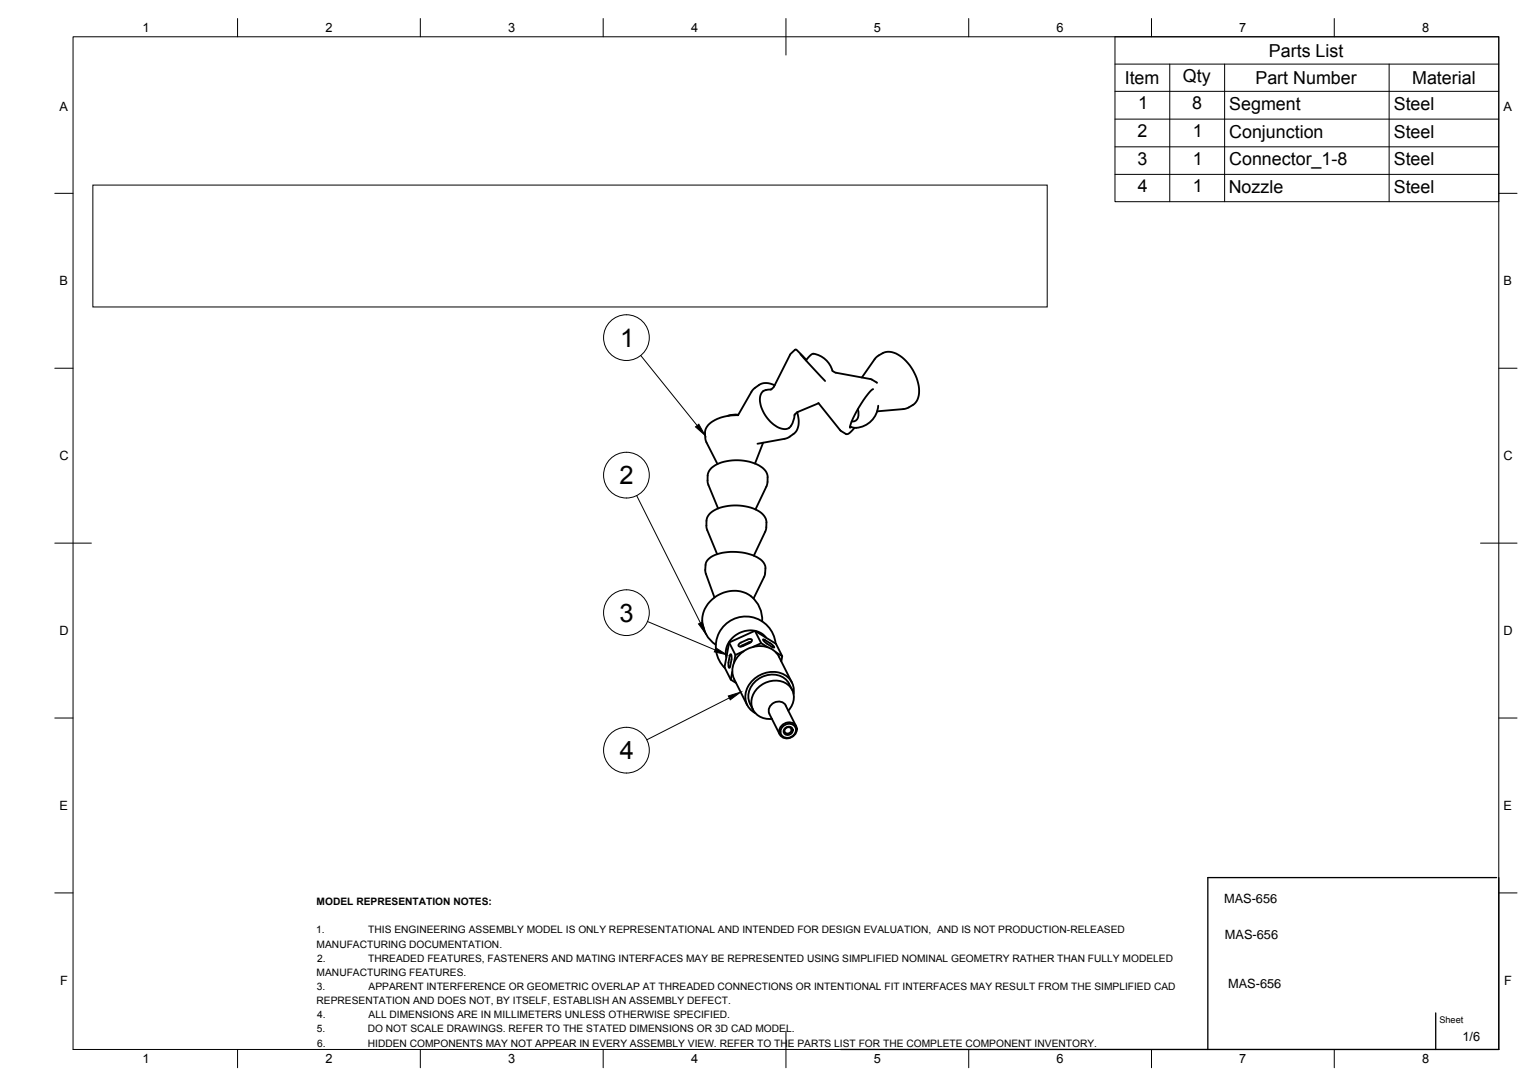
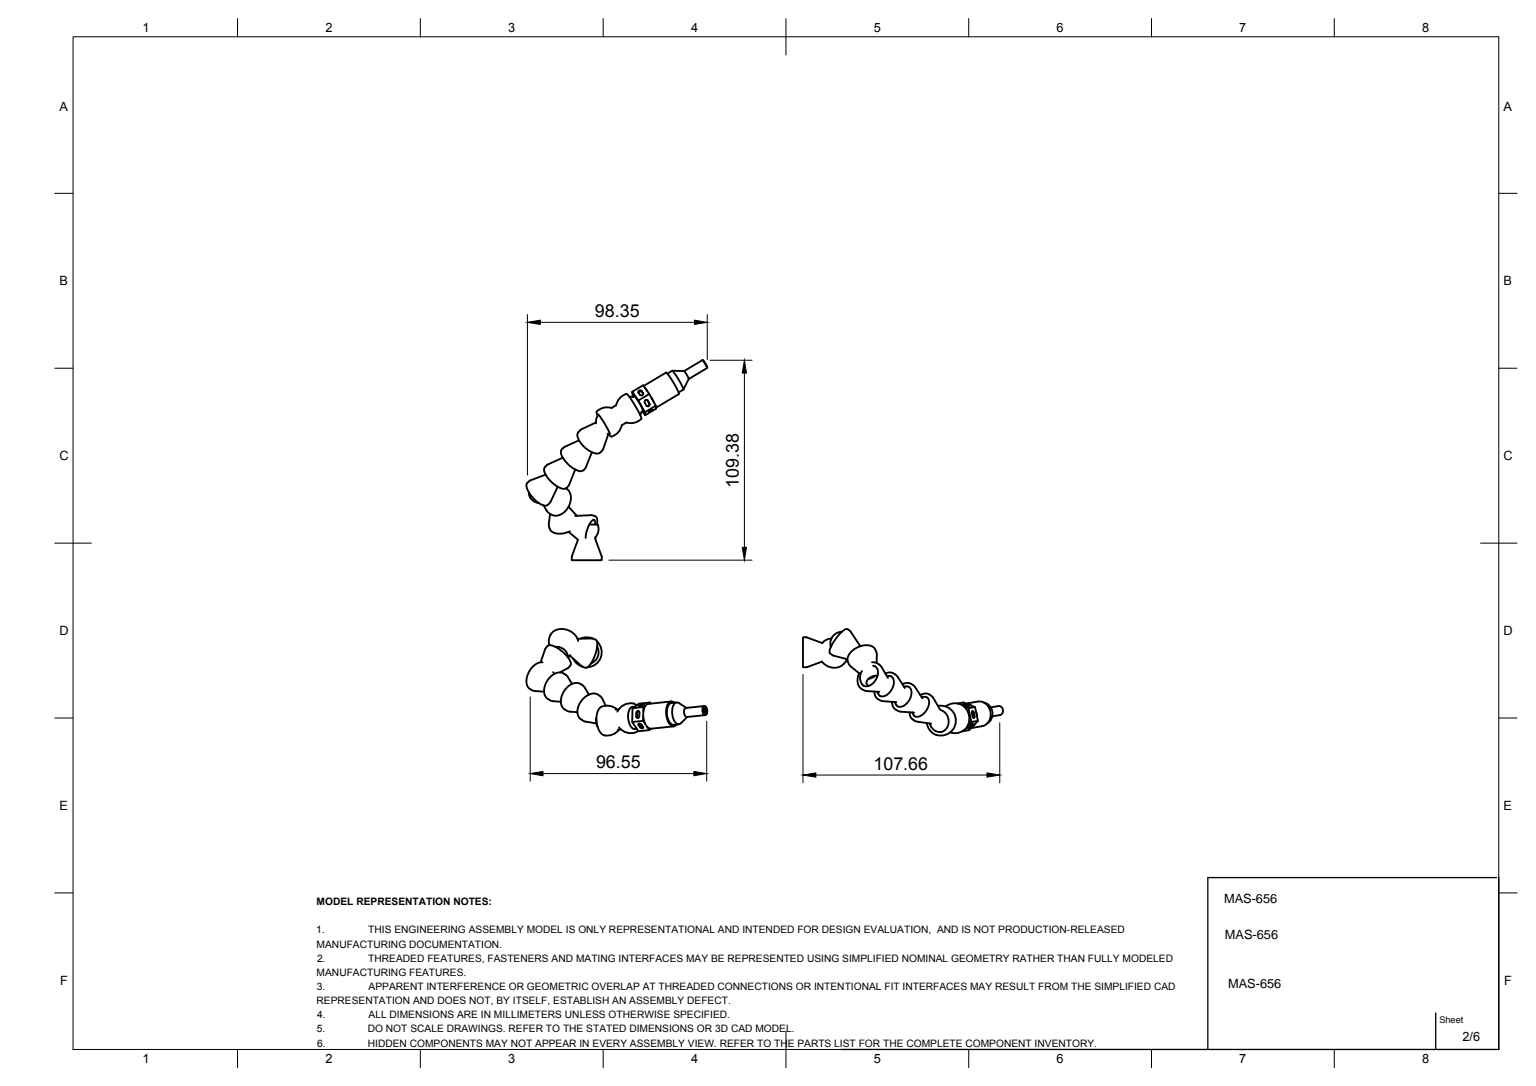
ISO-10303-21;
HEADER;
FILE_DESCRIPTION((''),'2;1');
FILE_NAME('MAS-656','2026-10-09T09:41:22-07:00',(''),(''),'','','');
FILE_SCHEMA (('AUTOMOTIVE_DESIGN { 1 0 10303 214 3 1 1 }'));
ENDSEC;
DATA;
#10 = MECHANICAL_DESIGN_GEOMETRIC_PRESENTATION_REPRESENTATION('',(#73,#74,
#75,#76,#77,#78),#4304) ;
#11 = ITEM_DEFINED_TRANSFORMATION($,$,#2468,#2519) ;
#12 = ITEM_DEFINED_TRANSFORMATION($,$,#2214,#2520) ;
#13 = ITEM_DEFINED_TRANSFORMATION($,$,#2268,#2521) ;
#14 = ITEM_DEFINED_TRANSFORMATION($,$,#2366,#2522) ;
#15 = ITEM_DEFINED_TRANSFORMATION($,$,#2468,#2523) ;
#16 = ITEM_DEFINED_TRANSFORMATION($,$,#2468,#2524) ;
#17 = ITEM_DEFINED_TRANSFORMATION($,$,#2468,#2525) ;
#18 = ITEM_DEFINED_TRANSFORMATION($,$,#2468,#2526) ;
#19 = ITEM_DEFINED_TRANSFORMATION($,$,#2468,#2527) ;
#20 = ITEM_DEFINED_TRANSFORMATION($,$,#2468,#2528) ;
#21 = ITEM_DEFINED_TRANSFORMATION($,$,#2468,#2529) ;
#22 = (
REPRESENTATION_RELATIONSHIP($,$,#4334,#4330)
REPRESENTATION_RELATIONSHIP_WITH_TRANSFORMATION(#11)
SHAPE_REPRESENTATION_RELATIONSHIP()
) ;
#23 = (
REPRESENTATION_RELATIONSHIP($,$,#4331,#4330)
REPRESENTATION_RELATIONSHIP_WITH_TRANSFORMATION(#12)
SHAPE_REPRESENTATION_RELATIONSHIP()
) ;
#24 = (
REPRESENTATION_RELATIONSHIP($,$,#4332,#4330)
REPRESENTATION_RELATIONSHIP_WITH_TRANSFORMATION(#13)
SHAPE_REPRESENTATION_RELATIONSHIP()
) ;
#25 = (
REPRESENTATION_RELATIONSHIP($,$,#4333,#4330)
REPRESENTATION_RELATIONSHIP_WITH_TRANSFORMATION(#14)
SHAPE_REPRESENTATION_RELATIONSHIP()
) ;
#26 = (
REPRESENTATION_RELATIONSHIP($,$,#4334,#4330)
REPRESENTATION_RELATIONSHIP_WITH_TRANSFORMATION(#15)
SHAPE_REPRESENTATION_RELATIONSHIP()
) ;
#27 = (
REPRESENTATION_RELATIONSHIP($,$,#4334,#4330)
REPRESENTATION_RELATIONSHIP_WITH_TRANSFORMATION(#16)
SHAPE_REPRESENTATION_RELATIONSHIP()
) ;
#28 = (
REPRESENTATION_RELATIONSHIP($,$,#4334,#4330)
REPRESENTATION_RELATIONSHIP_WITH_TRANSFORMATION(#17)
SHAPE_REPRESENTATION_RELATIONSHIP()
) ;
#29 = (
REPRESENTATION_RELATIONSHIP($,$,#4334,#4330)
REPRESENTATION_RELATIONSHIP_WITH_TRANSFORMATION(#18)
SHAPE_REPRESENTATION_RELATIONSHIP()
) ;
#30 = (
REPRESENTATION_RELATIONSHIP($,$,#4334,#4330)
REPRESENTATION_RELATIONSHIP_WITH_TRANSFORMATION(#19)
SHAPE_REPRESENTATION_RELATIONSHIP()
) ;
#31 = (
REPRESENTATION_RELATIONSHIP($,$,#4334,#4330)
REPRESENTATION_RELATIONSHIP_WITH_TRANSFORMATION(#20)
SHAPE_REPRESENTATION_RELATIONSHIP()
) ;
#32 = (
REPRESENTATION_RELATIONSHIP($,$,#4334,#4330)
REPRESENTATION_RELATIONSHIP_WITH_TRANSFORMATION(#21)
SHAPE_REPRESENTATION_RELATIONSHIP()
) ;
#33 = CONTEXT_DEPENDENT_SHAPE_REPRESENTATION(#22,#4319) ;
#34 = CONTEXT_DEPENDENT_SHAPE_REPRESENTATION(#23,#4320) ;
#35 = CONTEXT_DEPENDENT_SHAPE_REPRESENTATION(#24,#4321) ;
#36 = CONTEXT_DEPENDENT_SHAPE_REPRESENTATION(#25,#4322) ;
#37 = CONTEXT_DEPENDENT_SHAPE_REPRESENTATION(#26,#4323) ;
#38 = CONTEXT_DEPENDENT_SHAPE_REPRESENTATION(#27,#4324) ;
#39 = CONTEXT_DEPENDENT_SHAPE_REPRESENTATION(#28,#4325) ;
#40 = CONTEXT_DEPENDENT_SHAPE_REPRESENTATION(#29,#4326) ;
#41 = CONTEXT_DEPENDENT_SHAPE_REPRESENTATION(#30,#4327) ;
#42 = CONTEXT_DEPENDENT_SHAPE_REPRESENTATION(#31,#4328) ;
#43 = CONTEXT_DEPENDENT_SHAPE_REPRESENTATION(#32,#4329) ;
#44 = NEXT_ASSEMBLY_USAGE_OCCURRENCE('Segment:1','Segment:1','Segment:1',
#4336,#4340,'Segment:1') ;
#45 = NEXT_ASSEMBLY_USAGE_OCCURRENCE('Conjunction:1','Conjunction:1',
'Conjunction:1',#4336,#4337,'Conjunction:1') ;
#46 = NEXT_ASSEMBLY_USAGE_OCCURRENCE('Connector_1-8:1','Connector_1-8:1',
'Connector_1-8:1',#4336,#4338,'Connector_1-8:1') ;
#47 = NEXT_ASSEMBLY_USAGE_OCCURRENCE('Nozzle:1','Nozzle:1','Nozzle:1',#4336,
#4339,'Nozzle:1') ;
#48 = NEXT_ASSEMBLY_USAGE_OCCURRENCE('Segment:2','Segment:2','Segment:2',
#4336,#4340,'Segment:2') ;
#49 = NEXT_ASSEMBLY_USAGE_OCCURRENCE('Segment:3','Segment:3','Segment:3',
#4336,#4340,'Segment:3') ;
#50 = NEXT_ASSEMBLY_USAGE_OCCURRENCE('Segment:4','Segment:4','Segment:4',
#4336,#4340,'Segment:4') ;
#51 = NEXT_ASSEMBLY_USAGE_OCCURRENCE('Segment:5','Segment:5','Segment:5',
#4336,#4340,'Segment:5') ;
#52 = NEXT_ASSEMBLY_USAGE_OCCURRENCE('Segment:6','Segment:6','Segment:6',
#4336,#4340,'Segment:6') ;
#53 = NEXT_ASSEMBLY_USAGE_OCCURRENCE('Segment:7','Segment:7','Segment:7',
#4336,#4340,'Segment:7') ;
#54 = NEXT_ASSEMBLY_USAGE_OCCURRENCE('Segment:8','Segment:8','Segment:8',
#4336,#4340,'Segment:8') ;
#55 = B_SPLINE_SURFACE_WITH_KNOTS('',5,4,((#3896,#3897,#3898,#3899,#3900),
(#3901,#3902,#3903,#3904,#3905),(#3906,#3907,#3908,#3909,#3910),(#3911,
#3912,#3913,#3914,#3915),(#3916,#3917,#3918,#3919,#3920),(#3921,#3922,#3923,
#3924,#3925),(#3926,#3927,#3928,#3929,#3930),(#3931,#3932,#3933,#3934,#3935),
(#3936,#3937,#3938,#3939,#3940)),.UNSPECIFIED.,.F.,.F.,.F.,(6,3,6),(5,5),
(0.,2.00592385339,5.72401149719),(0.,4.),.UNSPECIFIED.) ;
#56 = B_SPLINE_SURFACE_WITH_KNOTS('',5,4,((#4027,#4028,#4029,#4030,#4031),
(#4032,#4033,#4034,#4035,#4036),(#4037,#4038,#4039,#4040,#4041),(#4042,
#4043,#4044,#4045,#4046),(#4047,#4048,#4049,#4050,#4051),(#4052,#4053,#4054,
#4055,#4056),(#4057,#4058,#4059,#4060,#4061),(#4062,#4063,#4064,#4065,#4066),
(#4067,#4068,#4069,#4070,#4071)),.UNSPECIFIED.,.F.,.F.,.F.,(6,3,6),(5,5),
(1.14412490986064,4.56688370431,6.86913676329339),(0.,4.0003840073707),
 .UNSPECIFIED.) ;
#57 = B_SPLINE_SURFACE_WITH_KNOTS('',5,4,((#4097,#4098,#4099,#4100,#4101),
(#4102,#4103,#4104,#4105,#4106),(#4107,#4108,#4109,#4110,#4111),(#4112,
#4113,#4114,#4115,#4116),(#4117,#4118,#4119,#4120,#4121),(#4122,#4123,#4124,
#4125,#4126),(#4127,#4128,#4129,#4130,#4131),(#4132,#4133,#4134,#4135,#4136),
(#4137,#4138,#4139,#4140,#4141)),.UNSPECIFIED.,.F.,.F.,.F.,(6,3,6),(5,5),
(1.81018607984298,7.54013629429,10.8709669414987),(-0.00161299974885553,
4.75),.UNSPECIFIED.) ;
#58 = B_SPLINE_SURFACE_WITH_KNOTS('',5,4,((#4144,#4145,#4146,#4147,#4148),
(#4149,#4150,#4151,#4152,#4153),(#4154,#4155,#4156,#4157,#4158),(#4159,
#4160,#4161,#4162,#4163),(#4164,#4165,#4166,#4167,#4168),(#4169,#4170,#4171,
#4172,#4173),(#4174,#4175,#4176,#4177,#4178),(#4179,#4180,#4181,#4182,#4183),
(#4184,#4185,#4186,#4187,#4188)),.UNSPECIFIED.,.F.,.F.,.F.,(6,3,6),(5,5),
(-0.00098737241999752,3.59707184609,9.05850997001312),(-0.000987383514799894,
4.75),.UNSPECIFIED.) ;
#59 = B_SPLINE_CURVE_WITH_KNOTS('',3,(#3693,#3694,#3695,#3696,#3697,#3698,
#3699,#3700,#3701,#3702,#3703,#3704,#3705,#3706,#3707,#3708,#3709,#3710,
#3711,#3712,#3713,#3714,#3715,#3716,#3717,#3718,#3719,#3720,#3721,#3722,
#3723,#3724,#3725,#3726,#3727,#3728,#3729,#3730),.UNSPECIFIED.,.T.,.F.,
(4,2,2,2,2,2,2,2,2,2,2,2,2,2,2,2,2,2,4),(-0.21266959393403,-0.197090411624007,
-0.181511229313983,-0.168315271544833,-0.161717292660258,-0.155119313775684,
-0.14852133489111,-0.141923356006537,-0.128727398237391,-0.113148215927359,
-0.0975690336173277,-0.0833467314908787,-0.0691244293644297,-0.058954473086547,
-0.0487845168086643,-0.0386145605307833,-0.0284446042529024,-0.0142223021264512,
0.),.UNSPECIFIED.) ;
#60 = B_SPLINE_CURVE_WITH_KNOTS('',3,(#3784,#3785,#3786,#3787,#3788,#3789,
#3790,#3791,#3792,#3793,#3794,#3795,#3796,#3797,#3798,#3799,#3800,#3801,
#3802,#3803,#3804,#3805),.UNSPECIFIED.,.F.,.F.,(4,2,2,2,2,2,2,2,2,2,4),
(-0.189267865923668,-0.181511229313965,-0.168315271544809,-0.16171729266023,
-0.155119313775652,-0.148521334891079,-0.141923356006506,-0.128727398237361,
-0.113148215927333,-0.0975690336173056,-0.0836220155565862),
 .UNSPECIFIED.) ;
#61 = B_SPLINE_CURVE_WITH_KNOTS('',3,(#3806,#3807,#3808,#3809,#3810,#3811,
#3812,#3813,#3814,#3815,#3816,#3817,#3818,#3819,#3820,#3821,#3822,#3823,
#3824,#3825,#3826,#3827,#3828),.UNSPECIFIED.,.F.,.F.,(4,2,2,2,2,2,2,2,3,
2,4),(-0.0836220155565862,-0.0833467314908613,-0.069124429364417,-0.0589544730865346,
-0.0487845168086522,-0.0386145605307738,-0.0284446042528953,-0.0142223021264476,
0.,0.0155791823100317,0.0234017280103608),.UNSPECIFIED.) ;
#62 = B_SPLINE_CURVE_WITH_KNOTS('',3,(#3831,#3832,#3833,#3834,#3835,#3836,
#3837,#3838,#3839,#3840,#3841,#3842,#3843,#3844,#3845,#3846,#3847,#3848,
#3849,#3850,#3851,#3852),.UNSPECIFIED.,.F.,.F.,(4,2,2,2,2,2,2,2,2,2,4),
(-0.189267865923044,-0.181511229313986,-0.16831527154483,-0.161717292660252,
-0.155119313775674,-0.148521334891098,-0.141923356006522,-0.128727398237371,
-0.113148215927341,-0.0975690336173107,-0.083622015556521),
 .UNSPECIFIED.) ;
#63 = B_SPLINE_CURVE_WITH_KNOTS('',3,(#3853,#3854,#3855,#3856,#3857,#3858,
#3859,#3860,#3861,#3862,#3863,#3864,#3865,#3866,#3867,#3868,#3869,#3870,
#3871,#3872,#3873,#3874,#3875),.UNSPECIFIED.,.F.,.F.,(4,2,2,2,2,2,2,2,3,
2,4),(-0.083622015556521,-0.0833467314908633,-0.0691244293644159,-0.0589544730865369,
-0.0487845168086579,-0.0386145605307766,-0.0284446042528953,-0.0142223021264477,
0.,0.0155791823100287,0.0234017280109999),.UNSPECIFIED.) ;
#64 = B_SPLINE_CURVE_WITH_KNOTS('',3,(#3943,#3944,#3945,#3946,#3947,#3948,
#3949,#3950,#3951,#3952,#3953,#3954,#3955,#3956,#3957,#3958,#3959,#3960,
#3961,#3962,#3963,#3964,#3965,#3966,#3967,#3968,#3969,#3970,#3971,#3972,
#3973,#3974,#3975,#3976,#3977,#3978,#3979,#3980,#3981,#3982,#3983,#3984,
#3985,#3986,#3987,#3988,#3989,#3990,#3991,#3992,#3993,#3994,#3995,#3996,
#3997,#3998,#3999,#4000,#4001,#4002,#4003,#4004,#4005,#4006,#4007,#4008,
#4009,#4010,#4011,#4012,#4013,#4014,#4015,#4016,#4017,#4018,#4019,#4020,
#4021,#4022,#4023,#4024),.UNSPECIFIED.,.F.,.F.,(4,3,3,3,3,3,3,3,3,3,3,3,
3,3,3,3,3,3,3,3,3,3,3,3,3,3,3,4),(0.,0.225460129220956,0.453336599536279,
0.681938236445323,0.91060483211705,1.13866755087004,1.36461264231086,1.58819548811847,
1.8099184881743,2.00592385339,2.22254168431687,2.44222941463765,2.66492844656066,
2.89048514085975,3.12062538022778,3.35076561959582,3.58299027924597,3.81573661936679,
4.04792384057385,4.27908578852667,4.50801790131295,4.57308155019,4.80116409571626,
5.02706122822092,5.25295836072559,5.47141386284307,5.68615166673345,5.72401149719),
 .UNSPECIFIED.) ;
#65 = SHAPE_REPRESENTATION_RELATIONSHIP('SRR','None',#4331,#69) ;
#66 = SHAPE_REPRESENTATION_RELATIONSHIP('SRR','None',#4332,#70) ;
#67 = SHAPE_REPRESENTATION_RELATIONSHIP('SRR','None',#4333,#71) ;
#68 = SHAPE_REPRESENTATION_RELATIONSHIP('SRR','None',#4334,#72) ;
#69 = ADVANCED_BREP_SHAPE_REPRESENTATION('',(#79),#4300) ;
#70 = ADVANCED_BREP_SHAPE_REPRESENTATION('',(#80),#4301) ;
#71 = ADVANCED_BREP_SHAPE_REPRESENTATION('',(#81,#82,#83),#4302) ;
#72 = ADVANCED_BREP_SHAPE_REPRESENTATION('',(#84),#4303) ;
#73 = STYLED_ITEM('',(#4360),#79) ;
#74 = STYLED_ITEM('',(#4360),#80) ;
#75 = STYLED_ITEM('',(#4360),#81) ;
#76 = STYLED_ITEM('',(#4360),#82) ;
#77 = STYLED_ITEM('',(#4361),#83) ;
#78 = STYLED_ITEM('',(#4362),#84) ;
#79 = MANIFOLD_SOLID_BREP('Body1',#2162) ;
#80 = MANIFOLD_SOLID_BREP('Body1',#2163) ;
#81 = MANIFOLD_SOLID_BREP('Body1',#2164) ;
#82 = MANIFOLD_SOLID_BREP('Body2',#2165) ;
#83 = MANIFOLD_SOLID_BREP('Body3',#2166) ;
#84 = MANIFOLD_SOLID_BREP('Body1',#2167) ;
#85 = FACE_BOUND('',#630,.T.) ;
#86 = FACE_BOUND('',#634,.T.) ;
#87 = FACE_BOUND('',#638,.T.) ;
#88 = FACE_BOUND('',#644,.T.) ;
#89 = FACE_BOUND('',#648,.T.) ;
#90 = FACE_BOUND('',#650,.T.) ;
#91 = FACE_BOUND('',#652,.T.) ;
#92 = FACE_BOUND('',#659,.T.) ;
#93 = FACE_BOUND('',#661,.T.) ;
#94 = FACE_BOUND('',#663,.T.) ;
#95 = FACE_BOUND('',#665,.T.) ;
#96 = FACE_BOUND('',#667,.T.) ;
#97 = FACE_BOUND('',#694,.T.) ;
#98 = FACE_BOUND('',#714,.T.) ;
#99 = FACE_BOUND('',#716,.T.) ;
#100 = FACE_BOUND('',#718,.T.) ;
#101 = FACE_BOUND('',#720,.T.) ;
#102 = FACE_BOUND('',#724,.T.) ;
#103 = FACE_BOUND('',#728,.T.) ;
#104 = FACE_BOUND('',#732,.T.) ;
#105 = FACE_BOUND('',#735,.T.) ;
#106 = FACE_BOUND('',#738,.T.) ;
#107 = FACE_BOUND('',#739,.T.) ;
#108 = FACE_BOUND('',#740,.T.) ;
#109 = FACE_BOUND('',#741,.T.) ;
#110 = FACE_BOUND('',#743,.T.) ;
#111 = FACE_BOUND('',#744,.T.) ;
#112 = FACE_BOUND('',#745,.T.) ;
#113 = FACE_BOUND('',#749,.T.) ;
#114 = FACE_BOUND('',#751,.T.) ;
#115 = FACE_BOUND('',#770,.T.) ;
#116 = FACE_BOUND('',#782,.T.) ;
#117 = PLANE('',#2257) ;
#118 = PLANE('',#2264) ;
#119 = PLANE('',#2272) ;
#120 = PLANE('',#2282) ;
#121 = PLANE('',#2288) ;
#122 = PLANE('',#2289) ;
#123 = PLANE('',#2291) ;
#124 = PLANE('',#2296) ;
#125 = PLANE('',#2297) ;
#126 = PLANE('',#2298) ;
#127 = PLANE('',#2301) ;
#128 = PLANE('',#2304) ;
#129 = PLANE('',#2307) ;
#130 = PLANE('',#2310) ;
#131 = PLANE('',#2313) ;
#132 = PLANE('',#2318) ;
#133 = PLANE('',#2319) ;
#134 = PLANE('',#2320) ;
#135 = PLANE('',#2325) ;
#136 = PLANE('',#2326) ;
#137 = PLANE('',#2327) ;
#138 = PLANE('',#2332) ;
#139 = PLANE('',#2333) ;
#140 = PLANE('',#2334) ;
#141 = PLANE('',#2339) ;
#142 = PLANE('',#2340) ;
#143 = PLANE('',#2341) ;
#144 = PLANE('',#2346) ;
#145 = PLANE('',#2347) ;
#146 = PLANE('',#2348) ;
#147 = PLANE('',#2351) ;
#148 = PLANE('',#2399) ;
#149 = PLANE('',#2400) ;
#150 = PLANE('',#2401) ;
#151 = PLANE('',#2402) ;
#152 = PLANE('',#2408) ;
#153 = PLANE('',#2414) ;
#154 = PLANE('',#2421) ;
#155 = PLANE('',#2425) ;
#156 = PLANE('',#2429) ;
#157 = PLANE('',#2435) ;
#158 = PLANE('',#2438) ;
#159 = PLANE('',#2481) ;
#160 = PLANE('',#2515) ;
#161 = TOROIDAL_SURFACE('',#2228,7.69960814153059,0.300000000000023) ;
#162 = TOROIDAL_SURFACE('',#2233,7.69960814153059,0.300000000000023) ;
#163 = TOROIDAL_SURFACE('',#2242,5.80000000000044,0.300000000000023) ;
#164 = TOROIDAL_SURFACE('',#2253,5.80000000000044,0.300000000000023) ;
#165 = TOROIDAL_SURFACE('',#2259,6.31637147335048,0.200000000000015) ;
#166 = TOROIDAL_SURFACE('',#2266,6.31637147335048,0.200000000000015) ;
#167 = TOROIDAL_SURFACE('',#2353,5.79274121460044,0.300000000000023) ;
#168 = TOROIDAL_SURFACE('',#2364,5.00000000000038,0.300000000000023) ;
#169 = TOROIDAL_SURFACE('',#2450,6.00000000000046,4.0000000000003) ;
#170 = TOROIDAL_SURFACE('',#2466,6.00000000000046,4.75000000000036) ;
#171 = TOROIDAL_SURFACE('',#2483,5.7927412146,0.3) ;
#172 = TOROIDAL_SURFACE('',#2491,5.,0.3) ;
#173 = TOROIDAL_SURFACE('',#2498,5.7,1.) ;
#174 = TOROIDAL_SURFACE('',#2502,7.9,0.3) ;
#175 = TOROIDAL_SURFACE('',#2511,7.2,1.) ;
#176 = TOROIDAL_SURFACE('',#2517,6.35142259969,0.2) ;
#177 = CYLINDRICAL_SURFACE('',#2221,3.00000000000023) ;
#178 = CYLINDRICAL_SURFACE('',#2250,5.50000000000042) ;
#179 = CYLINDRICAL_SURFACE('',#2255,6.11637147335047) ;
#180 = CYLINDRICAL_SURFACE('',#2261,6.11637147335047) ;
#181 = CYLINDRICAL_SURFACE('',#2274,4.86400000000037) ;
#182 = CYLINDRICAL_SURFACE('',#2276,3.00000000000023) ;
#183 = CYLINDRICAL_SURFACE('',#2284,4.10000000000031) ;
#184 = CYLINDRICAL_SURFACE('',#2286,4.86400000000037) ;
#185 = CYLINDRICAL_SURFACE('',#2294,1.00000000000008) ;
#186 = CYLINDRICAL_SURFACE('',#2300,1.00000000000008) ;
#187 = CYLINDRICAL_SURFACE('',#2316,1.00000000000008) ;
#188 = CYLINDRICAL_SURFACE('',#2322,1.00000000000008) ;
#189 = CYLINDRICAL_SURFACE('',#2323,1.00000000000008) ;
#190 = CYLINDRICAL_SURFACE('',#2329,1.00000000000008) ;
#191 = CYLINDRICAL_SURFACE('',#2330,1.00000000000008) ;
#192 = CYLINDRICAL_SURFACE('',#2336,1.00000000000008) ;
#193 = CYLINDRICAL_SURFACE('',#2337,1.00000000000008) ;
#194 = CYLINDRICAL_SURFACE('',#2343,1.00000000000008) ;
#195 = CYLINDRICAL_SURFACE('',#2344,1.00000000000008) ;
#196 = CYLINDRICAL_SURFACE('',#2350,1.00000000000008) ;
#197 = CYLINDRICAL_SURFACE('',#2357,4.70000000000036) ;
#198 = CYLINDRICAL_SURFACE('',#2367,6.85000000000052) ;
#199 = CYLINDRICAL_SURFACE('',#2370,6.00000000000046) ;
#200 = CYLINDRICAL_SURFACE('',#2375,2.50000000000019) ;
#201 = CYLINDRICAL_SURFACE('',#2382,1.00000000000008) ;
#202 = CYLINDRICAL_SURFACE('',#2386,4.25000000000032) ;
#203 = CYLINDRICAL_SURFACE('',#2391,4.28300000000033) ;
#204 = CYLINDRICAL_SURFACE('',#2395,5.00000000000038) ;
#205 = CYLINDRICAL_SURFACE('',#2403,0.300000000000023) ;
#206 = CYLINDRICAL_SURFACE('',#2405,1.3000000000001) ;
#207 = CYLINDRICAL_SURFACE('',#2412,0.300000000000023) ;
#208 = CYLINDRICAL_SURFACE('',#2416,0.850000000000065) ;
#209 = CYLINDRICAL_SURFACE('',#2418,3.55000000000027) ;
#210 = CYLINDRICAL_SURFACE('',#2423,4.25000000000032) ;
#211 = CYLINDRICAL_SURFACE('',#2427,3.00000000000023) ;
#212 = CYLINDRICAL_SURFACE('',#2433,0.300000000000023) ;
#213 = CYLINDRICAL_SURFACE('',#2434,0.300000000000023) ;
#214 = CYLINDRICAL_SURFACE('',#2441,1.3000000000001) ;
#215 = CYLINDRICAL_SURFACE('',#2447,2.00000000000015) ;
#216 = CYLINDRICAL_SURFACE('',#2454,2.05000000000016) ;
#217 = CYLINDRICAL_SURFACE('',#2462,1.2500000000001) ;
#218 = CYLINDRICAL_SURFACE('',#2469,4.1) ;
#219 = CYLINDRICAL_SURFACE('',#2474,3.) ;
#220 = CYLINDRICAL_SURFACE('',#2495,4.7) ;
#221 = CYLINDRICAL_SURFACE('',#2509,8.2) ;
#222 = CYLINDRICAL_SURFACE('',#2513,6.15142259969) ;
#223 = LINE('',#3294,#342) ;
#224 = LINE('',#3298,#343) ;
#225 = LINE('',#3301,#344) ;
#226 = LINE('',#3343,#345) ;
#227 = LINE('',#3351,#346) ;
#228 = LINE('',#3363,#347) ;
#229 = LINE('',#3374,#348) ;
#230 = LINE('',#3382,#349) ;
#231 = LINE('',#3385,#350) ;
#232 = LINE('',#3389,#351) ;
#233 = LINE('',#3393,#352) ;
#234 = LINE('',#3400,#353) ;
#235 = LINE('',#3405,#354) ;
#236 = LINE('',#3409,#355) ;
#237 = LINE('',#3411,#356) ;
#238 = LINE('',#3413,#357) ;
#239 = LINE('',#3415,#358) ;
#240 = LINE('',#3417,#359) ;
#241 = LINE('',#3418,#360) ;
#242 = LINE('',#3422,#361) ;
#243 = LINE('',#3424,#362) ;
#244 = LINE('',#3426,#363) ;
#245 = LINE('',#3428,#364) ;
#246 = LINE('',#3430,#365) ;
#247 = LINE('',#3431,#366) ;
#248 = LINE('',#3435,#367) ;
#249 = LINE('',#3436,#368) ;
#250 = LINE('',#3441,#369) ;
#251 = LINE('',#3444,#370) ;
#252 = LINE('',#3447,#371) ;
#253 = LINE('',#3449,#372) ;
#254 = LINE('',#3453,#373) ;
#255 = LINE('',#3454,#374) ;
#256 = LINE('',#3457,#375) ;
#257 = LINE('',#3458,#376) ;
#258 = LINE('',#3463,#377) ;
#259 = LINE('',#3466,#378) ;
#260 = LINE('',#3470,#379) ;
#261 = LINE('',#3473,#380) ;
#262 = LINE('',#3476,#381) ;
#263 = LINE('',#3480,#382) ;
#264 = LINE('',#3483,#383) ;
#265 = LINE('',#3486,#384) ;
#266 = LINE('',#3490,#385) ;
#267 = LINE('',#3493,#386) ;
#268 = LINE('',#3496,#387) ;
#269 = LINE('',#3500,#388) ;
#270 = LINE('',#3505,#389) ;
#271 = LINE('',#3509,#390) ;
#272 = LINE('',#3513,#391) ;
#273 = LINE('',#3515,#392) ;
#274 = LINE('',#3519,#393) ;
#275 = LINE('',#3520,#394) ;
#276 = LINE('',#3523,#395) ;
#277 = LINE('',#3524,#396) ;
#278 = LINE('',#3530,#397) ;
#279 = LINE('',#3532,#398) ;
#280 = LINE('',#3536,#399) ;
#281 = LINE('',#3537,#400) ;
#282 = LINE('',#3540,#401) ;
#283 = LINE('',#3541,#402) ;
#284 = LINE('',#3547,#403) ;
#285 = LINE('',#3549,#404) ;
#286 = LINE('',#3553,#405) ;
#287 = LINE('',#3554,#406) ;
#288 = LINE('',#3557,#407) ;
#289 = LINE('',#3558,#408) ;
#290 = LINE('',#3564,#409) ;
#291 = LINE('',#3566,#410) ;
#292 = LINE('',#3570,#411) ;
#293 = LINE('',#3571,#412) ;
#294 = LINE('',#3574,#413) ;
#295 = LINE('',#3575,#414) ;
#296 = LINE('',#3581,#415) ;
#297 = LINE('',#3583,#416) ;
#298 = LINE('',#3587,#417) ;
#299 = LINE('',#3588,#418) ;
#300 = LINE('',#3591,#419) ;
#301 = LINE('',#3592,#420) ;
#302 = LINE('',#3609,#421) ;
#303 = LINE('',#3624,#422) ;
#304 = LINE('',#3630,#423) ;
#305 = LINE('',#3634,#424) ;
#306 = LINE('',#3639,#425) ;
#307 = LINE('',#3642,#426) ;
#308 = LINE('',#3648,#427) ;
#309 = LINE('',#3653,#428) ;
#310 = LINE('',#3656,#429) ;
#311 = LINE('',#3661,#430) ;
#312 = LINE('',#3666,#431) ;
#313 = LINE('',#3671,#432) ;
#314 = LINE('',#3674,#433) ;
#315 = LINE('',#3679,#434) ;
#316 = LINE('',#3682,#435) ;
#317 = LINE('',#3692,#436) ;
#318 = LINE('',#3735,#437) ;
#319 = LINE('',#3743,#438) ;
#320 = LINE('',#3746,#439) ;
#321 = LINE('',#3753,#440) ;
#322 = LINE('',#3759,#441) ;
#323 = LINE('',#3766,#442) ;
#324 = LINE('',#3773,#443) ;
#325 = LINE('',#3781,#444) ;
#326 = LINE('',#3877,#445) ;
#327 = LINE('',#3879,#446) ;
#328 = LINE('',#3895,#447) ;
#329 = LINE('',#4077,#448) ;
#330 = LINE('',#4087,#449) ;
#331 = LINE('',#4096,#450) ;
#332 = LINE('',#4191,#451) ;
#333 = LINE('',#4196,#452) ;
#334 = LINE('',#4204,#453) ;
#335 = LINE('',#4209,#454) ;
#336 = LINE('',#4213,#455) ;
#337 = LINE('',#4216,#456) ;
#338 = LINE('',#4245,#457) ;
#339 = LINE('',#4266,#458) ;
#340 = LINE('',#4270,#459) ;
#341 = LINE('',#4276,#460) ;
#342 = VECTOR('',#2546,3.00000000000023) ;
#343 = VECTOR('',#2551,3.00000000000023) ;
#344 = VECTOR('',#2554,3.00000000000023) ;
#345 = VECTOR('',#2609,5.50000000000042) ;
#346 = VECTOR('',#2620,6.11637147335047) ;
#347 = VECTOR('',#2637,6.11637147335047) ;
#348 = VECTOR('',#2652,4.28300000000033) ;
#349 = VECTOR('',#2663,4.86400000000037) ;
#350 = VECTOR('',#2666,3.00000000000023) ;
#351 = VECTOR('',#2671,4.28300000000033) ;
#352 = VECTOR('',#2676,3.00000000000023) ;
#353 = VECTOR('',#2685,4.10000000000031) ;
#354 = VECTOR('',#2692,4.86400000000037) ;
#355 = VECTOR('',#2695,1.00000000000008) ;
#356 = VECTOR('',#2696,0.999999999999697) ;
#357 = VECTOR('',#2697,0.999999999999697) ;
#358 = VECTOR('',#2698,1.00000000000008) ;
#359 = VECTOR('',#2699,0.999999999999697) ;
#360 = VECTOR('',#2700,0.999999999999697) ;
#361 = VECTOR('',#2703,0.999999999999697) ;
#362 = VECTOR('',#2704,1.00000000000008) ;
#363 = VECTOR('',#2705,0.999999999999697) ;
#364 = VECTOR('',#2706,0.999999999999697) ;
#365 = VECTOR('',#2707,1.00000000000008) ;
#366 = VECTOR('',#2708,0.999999999999697) ;
#367 = VECTOR('',#2713,1.00000000000008) ;
#368 = VECTOR('',#2714,1.00000000000008) ;
#369 = VECTOR('',#2717,1.00000000000008) ;
#370 = VECTOR('',#2720,1.00000000000008) ;
#371 = VECTOR('',#2723,1.00000000000008) ;
#372 = VECTOR('',#2724,1.00000000000008) ;
#373 = VECTOR('',#2729,1.00000000000008) ;
#374 = VECTOR('',#2730,1.00000000000008) ;
#375 = VECTOR('',#2733,1.00000000000008) ;
#376 = VECTOR('',#2734,1.00000000000008) ;
#377 = VECTOR('',#2743,1.00000000000008) ;
#378 = VECTOR('',#2744,0.999999999999697) ;
#379 = VECTOR('',#2747,0.999999999999697) ;
#380 = VECTOR('',#2752,1.00000000000008) ;
#381 = VECTOR('',#2753,0.999999999999697) ;
#382 = VECTOR('',#2756,0.999999999999697) ;
#383 = VECTOR('',#2761,1.00000000000008) ;
#384 = VECTOR('',#2762,0.999999999999697) ;
#385 = VECTOR('',#2765,0.999999999999697) ;
#386 = VECTOR('',#2770,1.00000000000008) ;
#387 = VECTOR('',#2771,0.999999999999697) ;
#388 = VECTOR('',#2774,0.999999999999697) ;
#389 = VECTOR('',#2779,1.00000000000008) ;
#390 = VECTOR('',#2782,1.00000000000008) ;
#391 = VECTOR('',#2787,1.00000000000008) ;
#392 = VECTOR('',#2788,1.00000000000008) ;
#393 = VECTOR('',#2793,1.00000000000008) ;
#394 = VECTOR('',#2794,1.00000000000008) ;
#395 = VECTOR('',#2797,1.00000000000008) ;
#396 = VECTOR('',#2798,1.00000000000008) ;
#397 = VECTOR('',#2807,0.999999999999697) ;
#398 = VECTOR('',#2808,0.999999999999697) ;
#399 = VECTOR('',#2813,0.999999999999697) ;
#400 = VECTOR('',#2814,0.999999999999697) ;
#401 = VECTOR('',#2817,0.999999999999697) ;
#402 = VECTOR('',#2818,0.999999999999697) ;
#403 = VECTOR('',#2827,0.999999999999697) ;
#404 = VECTOR('',#2828,0.999999999999697) ;
#405 = VECTOR('',#2833,0.999999999999697) ;
#406 = VECTOR('',#2834,0.999999999999697) ;
#407 = VECTOR('',#2837,0.999999999999697) ;
#408 = VECTOR('',#2838,0.999999999999697) ;
#409 = VECTOR('',#2847,0.999999999999696) ;
#410 = VECTOR('',#2848,0.999999999999696) ;
#411 = VECTOR('',#2853,0.999999999999696) ;
#412 = VECTOR('',#2854,0.999999999999697) ;
#413 = VECTOR('',#2857,0.999999999999696) ;
#414 = VECTOR('',#2858,0.999999999999697) ;
#415 = VECTOR('',#2867,0.999999999999696) ;
#416 = VECTOR('',#2868,0.999999999999696) ;
#417 = VECTOR('',#2873,0.999999999999696) ;
#418 = VECTOR('',#2874,0.999999999999697) ;
#419 = VECTOR('',#2877,0.999999999999696) ;
#420 = VECTOR('',#2878,0.999999999999697) ;
#421 = VECTOR('',#2901,4.70000000000036) ;
#422 = VECTOR('',#2922,6.85000000000052) ;
#423 = VECTOR('',#2929,6.00000000000046) ;
#424 = VECTOR('',#2934,2.50000000000019) ;
#425 = VECTOR('',#2941,2.50000000000019) ;
#426 = VECTOR('',#2944,2.20000000000017) ;
#427 = VECTOR('',#2951,1.00000000000008) ;
#428 = VECTOR('',#2958,1.00000000000008) ;
#429 = VECTOR('',#2961,1.00000000000008) ;
#430 = VECTOR('',#2968,4.25000000000032) ;
#431 = VECTOR('',#2973,4.28300000000033) ;
#432 = VECTOR('',#2980,4.28300000000033) ;
#433 = VECTOR('',#2983,4.28300000000033) ;
#434 = VECTOR('',#2990,5.00000000000038) ;
#435 = VECTOR('',#2993,5.00000000000038) ;
#436 = VECTOR('',#3008,0.300000000000023) ;
#437 = VECTOR('',#3013,1.3000000000001) ;
#438 = VECTOR('',#3024,0.300000000000023) ;
#439 = VECTOR('',#3027,0.300000000000023) ;
#440 = VECTOR('',#3036,0.850000000000065) ;
#441 = VECTOR('',#3043,3.55000000000027) ;
#442 = VECTOR('',#3052,4.25000000000032) ;
#443 = VECTOR('',#3061,3.00000000000023) ;
#444 = VECTOR('',#3072,0.850000000000065) ;
#445 = VECTOR('',#3075,0.300000000000023) ;
#446 = VECTOR('',#3078,0.300000000000023) ;
#447 = VECTOR('',#3097,1.3000000000001) ;
#448 = VECTOR('',#3108,2.00000000000015) ;
#449 = VECTOR('',#3121,2.05000000000016) ;
#450 = VECTOR('',#3132,2.00000000000015) ;
#451 = VECTOR('',#3139,1.2500000000001) ;
#452 = VECTOR('',#3146,1.2500000000001) ;
#453 = VECTOR('',#3157,4.1) ;
#454 = VECTOR('',#3164,3.) ;
#455 = VECTOR('',#3169,3.) ;
#456 = VECTOR('',#3172,3.) ;
#457 = VECTOR('',#3211,4.7) ;
#458 = VECTOR('',#3238,4.7) ;
#459 = VECTOR('',#3243,8.2) ;
#460 = VECTOR('',#3252,6.15142259969) ;
#461 = CONICAL_SURFACE('',#2219,3.00000000000023,0.785398163397) ;
#462 = CONICAL_SURFACE('',#2223,3.00000000000023,0.785398163397) ;
#463 = CONICAL_SURFACE('',#2269,4.28300000000033,1.0471975512) ;
#464 = CONICAL_SURFACE('',#2278,4.28300000000033,1.0471975512) ;
#465 = CONICAL_SURFACE('',#2280,3.00000000000023,0.785398163397) ;
#466 = CONICAL_SURFACE('',#2373,2.50000000000019,0.566729217524) ;
#467 = CONICAL_SURFACE('',#2377,2.20000000000017,0.785398163397) ;
#468 = CONICAL_SURFACE('',#2379,1.00000000000008,0.785398163397) ;
#469 = CONICAL_SURFACE('',#2384,1.00000000000008,0.610865238198) ;
#470 = CONICAL_SURFACE('',#2388,4.28300000000033,1.0471975512) ;
#471 = CONICAL_SURFACE('',#2393,4.28300000000033,1.0471975512) ;
#472 = CONICAL_SURFACE('',#2397,5.00000000000038,0.785398163397) ;
#473 = CONICAL_SURFACE('',#2410,0.300000000000023,0.785398163397) ;
#474 = CONICAL_SURFACE('',#2432,0.850000000000065,0.844153986113) ;
#475 = CONICAL_SURFACE('',#2457,2.00000000000015,0.0499583957219) ;
#476 = CONICAL_SURFACE('',#2464,1.2500000000001,0.0499583957219) ;
#477 = CONICAL_SURFACE('',#2472,3.,0.785398163397) ;
#478 = CONICAL_SURFACE('',#2476,3.,0.785398163397) ;
#479 = CONICAL_SURFACE('',#2507,4.7,0.352990387827) ;
#480 = FACE_OUTER_BOUND('',#616,.T.) ;
#481 = FACE_OUTER_BOUND('',#617,.T.) ;
#482 = FACE_OUTER_BOUND('',#618,.T.) ;
#483 = FACE_OUTER_BOUND('',#619,.T.) ;
#484 = FACE_OUTER_BOUND('',#620,.T.) ;
#485 = FACE_OUTER_BOUND('',#621,.T.) ;
#486 = FACE_OUTER_BOUND('',#622,.T.) ;
#487 = FACE_OUTER_BOUND('',#623,.T.) ;
#488 = FACE_OUTER_BOUND('',#624,.T.) ;
#489 = FACE_OUTER_BOUND('',#625,.T.) ;
#490 = FACE_OUTER_BOUND('',#626,.T.) ;
#491 = FACE_OUTER_BOUND('',#627,.T.) ;
#492 = FACE_OUTER_BOUND('',#628,.T.) ;
#493 = FACE_OUTER_BOUND('',#629,.T.) ;
#494 = FACE_OUTER_BOUND('',#631,.T.) ;
#495 = FACE_OUTER_BOUND('',#632,.T.) ;
#496 = FACE_OUTER_BOUND('',#633,.T.) ;
#497 = FACE_OUTER_BOUND('',#635,.T.) ;
#498 = FACE_OUTER_BOUND('',#636,.T.) ;
#499 = FACE_OUTER_BOUND('',#637,.T.) ;
#500 = FACE_OUTER_BOUND('',#639,.T.) ;
#501 = FACE_OUTER_BOUND('',#640,.T.) ;
#502 = FACE_OUTER_BOUND('',#641,.T.) ;
#503 = FACE_OUTER_BOUND('',#642,.T.) ;
#504 = FACE_OUTER_BOUND('',#643,.T.) ;
#505 = FACE_OUTER_BOUND('',#645,.T.) ;
#506 = FACE_OUTER_BOUND('',#646,.T.) ;
#507 = FACE_OUTER_BOUND('',#647,.T.) ;
#508 = FACE_OUTER_BOUND('',#649,.T.) ;
#509 = FACE_OUTER_BOUND('',#651,.T.) ;
#510 = FACE_OUTER_BOUND('',#653,.T.) ;
#511 = FACE_OUTER_BOUND('',#654,.T.) ;
#512 = FACE_OUTER_BOUND('',#655,.T.) ;
#513 = FACE_OUTER_BOUND('',#656,.T.) ;
#514 = FACE_OUTER_BOUND('',#657,.T.) ;
#515 = FACE_OUTER_BOUND('',#658,.T.) ;
#516 = FACE_OUTER_BOUND('',#660,.T.) ;
#517 = FACE_OUTER_BOUND('',#662,.T.) ;
#518 = FACE_OUTER_BOUND('',#664,.T.) ;
#519 = FACE_OUTER_BOUND('',#666,.T.) ;
#520 = FACE_OUTER_BOUND('',#668,.T.) ;
#521 = FACE_OUTER_BOUND('',#669,.T.) ;
#522 = FACE_OUTER_BOUND('',#670,.T.) ;
#523 = FACE_OUTER_BOUND('',#671,.T.) ;
#524 = FACE_OUTER_BOUND('',#672,.T.) ;
#525 = FACE_OUTER_BOUND('',#673,.T.) ;
#526 = FACE_OUTER_BOUND('',#674,.T.) ;
#527 = FACE_OUTER_BOUND('',#675,.T.) ;
#528 = FACE_OUTER_BOUND('',#676,.T.) ;
#529 = FACE_OUTER_BOUND('',#677,.T.) ;
#530 = FACE_OUTER_BOUND('',#678,.T.) ;
#531 = FACE_OUTER_BOUND('',#679,.T.) ;
#532 = FACE_OUTER_BOUND('',#680,.T.) ;
#533 = FACE_OUTER_BOUND('',#681,.T.) ;
#534 = FACE_OUTER_BOUND('',#682,.T.) ;
#535 = FACE_OUTER_BOUND('',#683,.T.) ;
#536 = FACE_OUTER_BOUND('',#684,.T.) ;
#537 = FACE_OUTER_BOUND('',#685,.T.) ;
#538 = FACE_OUTER_BOUND('',#686,.T.) ;
#539 = FACE_OUTER_BOUND('',#687,.T.) ;
#540 = FACE_OUTER_BOUND('',#688,.T.) ;
#541 = FACE_OUTER_BOUND('',#689,.T.) ;
#542 = FACE_OUTER_BOUND('',#690,.T.) ;
#543 = FACE_OUTER_BOUND('',#691,.T.) ;
#544 = FACE_OUTER_BOUND('',#692,.T.) ;
#545 = FACE_OUTER_BOUND('',#693,.T.) ;
#546 = FACE_OUTER_BOUND('',#695,.T.) ;
#547 = FACE_OUTER_BOUND('',#696,.T.) ;
#548 = FACE_OUTER_BOUND('',#697,.T.) ;
#549 = FACE_OUTER_BOUND('',#698,.T.) ;
#550 = FACE_OUTER_BOUND('',#699,.T.) ;
#551 = FACE_OUTER_BOUND('',#700,.T.) ;
#552 = FACE_OUTER_BOUND('',#701,.T.) ;
#553 = FACE_OUTER_BOUND('',#702,.T.) ;
#554 = FACE_OUTER_BOUND('',#703,.T.) ;
#555 = FACE_OUTER_BOUND('',#704,.T.) ;
#556 = FACE_OUTER_BOUND('',#705,.T.) ;
#557 = FACE_OUTER_BOUND('',#706,.T.) ;
#558 = FACE_OUTER_BOUND('',#707,.T.) ;
#559 = FACE_OUTER_BOUND('',#708,.T.) ;
#560 = FACE_OUTER_BOUND('',#709,.T.) ;
#561 = FACE_OUTER_BOUND('',#710,.T.) ;
#562 = FACE_OUTER_BOUND('',#711,.T.) ;
#563 = FACE_OUTER_BOUND('',#712,.T.) ;
#564 = FACE_OUTER_BOUND('',#713,.T.) ;
#565 = FACE_OUTER_BOUND('',#715,.T.) ;
#566 = FACE_OUTER_BOUND('',#717,.T.) ;
#567 = FACE_OUTER_BOUND('',#719,.T.) ;
#568 = FACE_OUTER_BOUND('',#721,.T.) ;
#569 = FACE_OUTER_BOUND('',#722,.T.) ;
#570 = FACE_OUTER_BOUND('',#723,.T.) ;
#571 = FACE_OUTER_BOUND('',#725,.T.) ;
#572 = FACE_OUTER_BOUND('',#726,.T.) ;
#573 = FACE_OUTER_BOUND('',#727,.T.) ;
#574 = FACE_OUTER_BOUND('',#729,.T.) ;
#575 = FACE_OUTER_BOUND('',#730,.T.) ;
#576 = FACE_OUTER_BOUND('',#731,.T.) ;
#577 = FACE_OUTER_BOUND('',#733,.T.) ;
#578 = FACE_OUTER_BOUND('',#734,.T.) ;
#579 = FACE_OUTER_BOUND('',#736,.T.) ;
#580 = FACE_OUTER_BOUND('',#737,.T.) ;
#581 = FACE_OUTER_BOUND('',#742,.T.) ;
#582 = FACE_OUTER_BOUND('',#746,.T.) ;
#583 = FACE_OUTER_BOUND('',#747,.T.) ;
#584 = FACE_OUTER_BOUND('',#748,.T.) ;
#585 = FACE_OUTER_BOUND('',#750,.T.) ;
#586 = FACE_OUTER_BOUND('',#752,.T.) ;
#587 = FACE_OUTER_BOUND('',#753,.T.) ;
#588 = FACE_OUTER_BOUND('',#754,.T.) ;
#589 = FACE_OUTER_BOUND('',#755,.T.) ;
#590 = FACE_OUTER_BOUND('',#756,.T.) ;
#591 = FACE_OUTER_BOUND('',#757,.T.) ;
#592 = FACE_OUTER_BOUND('',#758,.T.) ;
#593 = FACE_OUTER_BOUND('',#759,.T.) ;
#594 = FACE_OUTER_BOUND('',#760,.T.) ;
#595 = FACE_OUTER_BOUND('',#761,.T.) ;
#596 = FACE_OUTER_BOUND('',#762,.T.) ;
#597 = FACE_OUTER_BOUND('',#763,.T.) ;
#598 = FACE_OUTER_BOUND('',#764,.T.) ;
#599 = FACE_OUTER_BOUND('',#765,.T.) ;
#600 = FACE_OUTER_BOUND('',#766,.T.) ;
#601 = FACE_OUTER_BOUND('',#767,.T.) ;
#602 = FACE_OUTER_BOUND('',#768,.T.) ;
#603 = FACE_OUTER_BOUND('',#769,.T.) ;
#604 = FACE_OUTER_BOUND('',#771,.T.) ;
#605 = FACE_OUTER_BOUND('',#772,.T.) ;
#606 = FACE_OUTER_BOUND('',#773,.T.) ;
#607 = FACE_OUTER_BOUND('',#774,.T.) ;
#608 = FACE_OUTER_BOUND('',#775,.T.) ;
#609 = FACE_OUTER_BOUND('',#776,.T.) ;
#610 = FACE_OUTER_BOUND('',#777,.T.) ;
#611 = FACE_OUTER_BOUND('',#778,.T.) ;
#612 = FACE_OUTER_BOUND('',#779,.T.) ;
#613 = FACE_OUTER_BOUND('',#780,.T.) ;
#614 = FACE_OUTER_BOUND('',#781,.T.) ;
#615 = FACE_OUTER_BOUND('',#783,.T.) ;
#616 = EDGE_LOOP('',(#1431,#1432,#1433,#1434)) ;
#617 = EDGE_LOOP('',(#1435,#1436,#1437,#1438)) ;
#618 = EDGE_LOOP('',(#1439,#1440,#1441,#1442)) ;
#619 = EDGE_LOOP('',(#1443,#1444,#1445,#1446)) ;
#620 = EDGE_LOOP('',(#1447,#1448,#1449,#1450)) ;
#621 = EDGE_LOOP('',(#1451,#1452,#1453,#1454,#1455)) ;
#622 = EDGE_LOOP('',(#1456,#1457,#1458,#1459,#1460)) ;
#623 = EDGE_LOOP('',(#1461,#1462,#1463,#1464,#1465,#1466)) ;
#624 = EDGE_LOOP('',(#1467,#1468,#1469,#1470,#1471,#1472)) ;
#625 = EDGE_LOOP('',(#1473,#1474,#1475,#1476,#1477,#1478)) ;
#626 = EDGE_LOOP('',(#1479,#1480,#1481,#1482,#1483,#1484)) ;
#627 = EDGE_LOOP('',(#1485,#1486,#1487,#1488,#1489,#1490)) ;
#628 = EDGE_LOOP('',(#1491,#1492,#1493,#1494)) ;
#629 = EDGE_LOOP('',(#1495)) ;
#630 = EDGE_LOOP('',(#1496)) ;
#631 = EDGE_LOOP('',(#1497,#1498,#1499,#1500)) ;
#632 = EDGE_LOOP('',(#1501,#1502,#1503,#1504,#1505)) ;
#633 = EDGE_LOOP('',(#1506)) ;
#634 = EDGE_LOOP('',(#1507)) ;
#635 = EDGE_LOOP('',(#1508,#1509,#1510,#1511,#1512)) ;
#636 = EDGE_LOOP('',(#1513,#1514,#1515,#1516)) ;
#637 = EDGE_LOOP('',(#1517)) ;
#638 = EDGE_LOOP('',(#1518)) ;
#639 = EDGE_LOOP('',(#1519,#1520,#1521,#1522)) ;
#640 = EDGE_LOOP('',(#1523,#1524,#1525,#1526)) ;
#641 = EDGE_LOOP('',(#1527,#1528,#1529,#1530)) ;
#642 = EDGE_LOOP('',(#1531,#1532,#1533,#1534)) ;
#643 = EDGE_LOOP('',(#1535)) ;
#644 = EDGE_LOOP('',(#1536)) ;
#645 = EDGE_LOOP('',(#1537,#1538,#1539,#1540)) ;
#646 = EDGE_LOOP('',(#1541,#1542,#1543,#1544)) ;
#647 = EDGE_LOOP('',(#1545,#1546,#1547,#1548,#1549,#1550)) ;
#648 = EDGE_LOOP('',(#1551)) ;
#649 = EDGE_LOOP('',(#1552,#1553,#1554,#1555,#1556,#1557)) ;
#650 = EDGE_LOOP('',(#1558)) ;
#651 = EDGE_LOOP('',(#1559,#1560,#1561,#1562)) ;
#652 = EDGE_LOOP('',(#1563,#1564,#1565,#1566)) ;
#653 = EDGE_LOOP('',(#1567,#1568,#1569,#1570)) ;
#654 = EDGE_LOOP('',(#1571,#1572,#1573,#1574)) ;
#655 = EDGE_LOOP('',(#1575,#1576,#1577,#1578)) ;
#656 = EDGE_LOOP('',(#1579,#1580,#1581,#1582)) ;
#657 = EDGE_LOOP('',(#1583,#1584,#1585,#1586)) ;
#658 = EDGE_LOOP('',(#1587,#1588,#1589,#1590)) ;
#659 = EDGE_LOOP('',(#1591,#1592,#1593,#1594)) ;
#660 = EDGE_LOOP('',(#1595,#1596,#1597,#1598)) ;
#661 = EDGE_LOOP('',(#1599,#1600,#1601,#1602)) ;
#662 = EDGE_LOOP('',(#1603,#1604,#1605,#1606)) ;
#663 = EDGE_LOOP('',(#1607,#1608,#1609,#1610)) ;
#664 = EDGE_LOOP('',(#1611,#1612,#1613,#1614)) ;
#665 = EDGE_LOOP('',(#1615,#1616,#1617,#1618)) ;
#666 = EDGE_LOOP('',(#1619,#1620,#1621,#1622)) ;
#667 = EDGE_LOOP('',(#1623,#1624,#1625,#1626)) ;
#668 = EDGE_LOOP('',(#1627,#1628,#1629,#1630)) ;
#669 = EDGE_LOOP('',(#1631,#1632,#1633,#1634)) ;
#670 = EDGE_LOOP('',(#1635,#1636,#1637,#1638)) ;
#671 = EDGE_LOOP('',(#1639,#1640,#1641,#1642)) ;
#672 = EDGE_LOOP('',(#1643,#1644,#1645,#1646)) ;
#673 = EDGE_LOOP('',(#1647,#1648,#1649,#1650)) ;
#674 = EDGE_LOOP('',(#1651,#1652,#1653,#1654)) ;
#675 = EDGE_LOOP('',(#1655,#1656,#1657,#1658)) ;
#676 = EDGE_LOOP('',(#1659,#1660,#1661,#1662)) ;
#677 = EDGE_LOOP('',(#1663,#1664,#1665,#1666)) ;
#678 = EDGE_LOOP('',(#1667,#1668,#1669,#1670)) ;
#679 = EDGE_LOOP('',(#1671,#1672,#1673,#1674)) ;
#680 = EDGE_LOOP('',(#1675,#1676,#1677,#1678)) ;
#681 = EDGE_LOOP('',(#1679,#1680,#1681,#1682)) ;
#682 = EDGE_LOOP('',(#1683,#1684,#1685,#1686)) ;
#683 = EDGE_LOOP('',(#1687,#1688,#1689,#1690)) ;
#684 = EDGE_LOOP('',(#1691,#1692,#1693,#1694)) ;
#685 = EDGE_LOOP('',(#1695,#1696,#1697,#1698)) ;
#686 = EDGE_LOOP('',(#1699,#1700,#1701,#1702)) ;
#687 = EDGE_LOOP('',(#1703,#1704,#1705,#1706)) ;
#688 = EDGE_LOOP('',(#1707,#1708,#1709,#1710)) ;
#689 = EDGE_LOOP('',(#1711,#1712,#1713,#1714)) ;
#690 = EDGE_LOOP('',(#1715,#1716,#1717,#1718)) ;
#691 = EDGE_LOOP('',(#1719,#1720,#1721,#1722)) ;
#692 = EDGE_LOOP('',(#1723,#1724,#1725,#1726)) ;
#693 = EDGE_LOOP('',(#1727)) ;
#694 = EDGE_LOOP('',(#1728)) ;
#695 = EDGE_LOOP('',(#1729,#1730,#1731,#1732,#1733)) ;
#696 = EDGE_LOOP('',(#1734,#1735,#1736,#1737,#1738)) ;
#697 = EDGE_LOOP('',(#1739,#1740,#1741,#1742,#1743,#1744)) ;
#698 = EDGE_LOOP('',(#1745,#1746,#1747,#1748,#1749,#1750)) ;
#699 = EDGE_LOOP('',(#1751,#1752,#1753,#1754)) ;
#700 = EDGE_LOOP('',(#1755,#1756,#1757,#1758)) ;
#701 = EDGE_LOOP('',(#1759,#1760,#1761,#1762)) ;
#702 = EDGE_LOOP('',(#1763,#1764,#1765,#1766)) ;
#703 = EDGE_LOOP('',(#1767,#1768,#1769,#1770)) ;
#704 = EDGE_LOOP('',(#1771,#1772,#1773,#1774)) ;
#705 = EDGE_LOOP('',(#1775,#1776,#1777,#1778)) ;
#706 = EDGE_LOOP('',(#1779,#1780,#1781,#1782)) ;
#707 = EDGE_LOOP('',(#1783,#1784,#1785,#1786)) ;
#708 = EDGE_LOOP('',(#1787,#1788,#1789,#1790)) ;
#709 = EDGE_LOOP('',(#1791,#1792,#1793,#1794)) ;
#710 = EDGE_LOOP('',(#1795,#1796,#1797,#1798)) ;
#711 = EDGE_LOOP('',(#1799,#1800,#1801,#1802)) ;
#712 = EDGE_LOOP('',(#1803,#1804,#1805,#1806)) ;
#713 = EDGE_LOOP('',(#1807)) ;
#714 = EDGE_LOOP('',(#1808)) ;
#715 = EDGE_LOOP('',(#1809)) ;
#716 = EDGE_LOOP('',(#1810)) ;
#717 = EDGE_LOOP('',(#1811)) ;
#718 = EDGE_LOOP('',(#1812)) ;
#719 = EDGE_LOOP('',(#1813)) ;
#720 = EDGE_LOOP('',(#1814)) ;
#721 = EDGE_LOOP('',(#1815,#1816,#1817,#1818)) ;
#722 = EDGE_LOOP('',(#1819,#1820,#1821,#1822)) ;
#723 = EDGE_LOOP('',(#1823)) ;
#724 = EDGE_LOOP('',(#1824)) ;
#725 = EDGE_LOOP('',(#1825,#1826,#1827,#1828)) ;
#726 = EDGE_LOOP('',(#1829,#1830,#1831,#1832)) ;
#727 = EDGE_LOOP('',(#1833)) ;
#728 = EDGE_LOOP('',(#1834)) ;
#729 = EDGE_LOOP('',(#1835,#1836,#1837,#1838)) ;
#730 = EDGE_LOOP('',(#1839,#1840,#1841,#1842)) ;
#731 = EDGE_LOOP('',(#1843)) ;
#732 = EDGE_LOOP('',(#1844)) ;
#733 = EDGE_LOOP('',(#1845,#1846,#1847,#1848)) ;
#734 = EDGE_LOOP('',(#1849)) ;
#735 = EDGE_LOOP('',(#1850)) ;
#736 = EDGE_LOOP('',(#1851,#1852,#1853,#1854)) ;
#737 = EDGE_LOOP('',(#1855)) ;
#738 = EDGE_LOOP('',(#1856)) ;
#739 = EDGE_LOOP('',(#1857)) ;
#740 = EDGE_LOOP('',(#1858)) ;
#741 = EDGE_LOOP('',(#1859)) ;
#742 = EDGE_LOOP('',(#1860,#1861,#1862,#1863)) ;
#743 = EDGE_LOOP('',(#1864,#1865)) ;
#744 = EDGE_LOOP('',(#1866,#1867)) ;
#745 = EDGE_LOOP('',(#1868)) ;
#746 = EDGE_LOOP('',(#1869,#1870,#1871,#1872,#1873)) ;
#747 = EDGE_LOOP('',(#1874,#1875,#1876,#1877,#1878)) ;
#748 = EDGE_LOOP('',(#1879)) ;
#749 = EDGE_LOOP('',(#1880)) ;
#750 = EDGE_LOOP('',(#1881)) ;
#751 = EDGE_LOOP('',(#1882)) ;
#752 = EDGE_LOOP('',(#1883,#1884,#1885,#1886,#1887)) ;
#753 = EDGE_LOOP('',(#1888,#1889,#1890,#1891)) ;
#754 = EDGE_LOOP('',(#1892,#1893,#1894,#1895)) ;
#755 = EDGE_LOOP('',(#1896,#1897,#1898,#1899,#1900)) ;
#756 = EDGE_LOOP('',(#1901,#1902,#1903,#1904,#1905,#1906)) ;
#757 = EDGE_LOOP('',(#1907,#1908,#1909,#1910,#1911)) ;
#758 = EDGE_LOOP('',(#1912,#1913,#1914,#1915,#1916,#1917)) ;
#759 = EDGE_LOOP('',(#1918,#1919,#1920,#1921)) ;
#760 = EDGE_LOOP('',(#1922,#1923,#1924,#1925)) ;
#761 = EDGE_LOOP('',(#1926,#1927,#1928,#1929)) ;
#762 = EDGE_LOOP('',(#1930,#1931,#1932,#1933,#1934)) ;
#763 = EDGE_LOOP('',(#1935,#1936,#1937,#1938)) ;
#764 = EDGE_LOOP('',(#1939,#1940,#1941,#1942)) ;
#765 = EDGE_LOOP('',(#1943,#1944,#1945,#1946)) ;
#766 = EDGE_LOOP('',(#1947,#1948,#1949,#1950)) ;
#767 = EDGE_LOOP('',(#1951,#1952,#1953,#1954)) ;
#768 = EDGE_LOOP('',(#1955,#1956,#1957,#1958)) ;
#769 = EDGE_LOOP('',(#1959)) ;
#770 = EDGE_LOOP('',(#1960)) ;
#771 = EDGE_LOOP('',(#1961,#1962,#1963,#1964,#1965)) ;
#772 = EDGE_LOOP('',(#1966,#1967,#1968,#1969,#1970,#1971)) ;
#773 = EDGE_LOOP('',(#1972,#1973,#1974,#1975,#1976,#1977)) ;
#774 = EDGE_LOOP('',(#1978,#1979,#1980,#1981,#1982,#1983)) ;
#775 = EDGE_LOOP('',(#1984,#1985,#1986,#1987,#1988,#1989)) ;
#776 = EDGE_LOOP('',(#1990,#1991,#1992,#1993,#1994)) ;
#777 = EDGE_LOOP('',(#1995,#1996,#1997,#1998,#1999)) ;
#778 = EDGE_LOOP('',(#2000,#2001,#2002,#2003,#2004)) ;
#779 = EDGE_LOOP('',(#2005,#2006,#2007,#2008)) ;
#780 = EDGE_LOOP('',(#2009,#2010,#2011,#2012)) ;
#781 = EDGE_LOOP('',(#2013)) ;
#782 = EDGE_LOOP('',(#2014)) ;
#783 = EDGE_LOOP('',(#2015,#2016,#2017,#2018)) ;
#784 = CIRCLE('',#2216,4.59619407771035) ;
#785 = CIRCLE('',#2217,6.5000000000005) ;
#786 = CIRCLE('',#2218,6.11637147335047) ;
#787 = CIRCLE('',#2220,3.00000000000023) ;
#788 = CIRCLE('',#2222,3.00000000000023) ;
#789 = CIRCLE('',#2224,4.59619407771035) ;
#790 = CIRCLE('',#2226,6.11637147335047) ;
#791 = CIRCLE('',#2227,6.5000000000005) ;
#792 = CIRCLE('',#2229,7.69960814153059) ;
#793 = CIRCLE('',#2230,0.300000000000023) ;
#794 = CIRCLE('',#2231,7.99199832412061) ;
#795 = CIRCLE('',#2232,7.99199832412061) ;
#796 = CIRCLE('',#2234,7.99199832412061) ;
#797 = CIRCLE('',#2235,7.99199832412061) ;
#798 = CIRCLE('',#2236,0.300000000000023) ;
#799 = CIRCLE('',#2237,7.69960814153059) ;
#800 = CIRCLE('',#2239,8.20000000000061) ;
#801 = CIRCLE('',#2240,5.59529411765043) ;
#802 = CIRCLE('',#2241,5.59529411765043) ;
#803 = CIRCLE('',#2243,0.300000000000023) ;
#804 = CIRCLE('',#2244,5.50000000000042) ;
#805 = CIRCLE('',#2245,5.50000000000042) ;
#806 = CIRCLE('',#2247,5.59529411765043) ;
#807 = CIRCLE('',#2248,8.20000000000061) ;
#808 = CIRCLE('',#2249,5.59529411765043) ;
#809 = CIRCLE('',#2251,5.50000000000042) ;
#810 = CIRCLE('',#2252,5.50000000000042) ;
#811 = CIRCLE('',#2254,0.300000000000023) ;
#812 = CIRCLE('',#2256,6.11637147335047) ;
#813 = CIRCLE('',#2258,6.31637147335048) ;
#814 = CIRCLE('',#2260,0.200000000000015) ;
#815 = CIRCLE('',#2262,6.11637147335047) ;
#816 = CIRCLE('',#2263,6.11637147335047) ;
#817 = CIRCLE('',#2265,6.31637147335048) ;
#818 = CIRCLE('',#2267,0.200000000000015) ;
#819 = CIRCLE('',#2270,4.86400000000037) ;
#820 = CIRCLE('',#2271,4.28300000000033) ;
#821 = CIRCLE('',#2273,3.00000000000023) ;
#822 = CIRCLE('',#2275,4.86400000000037) ;
#823 = CIRCLE('',#2277,3.00000000000023) ;
#824 = CIRCLE('',#2279,4.28300000000033) ;
#825 = CIRCLE('',#2281,4.10000000000031) ;
#826 = CIRCLE('',#2283,4.86400000000037) ;
#827 = CIRCLE('',#2285,4.10000000000031) ;
#828 = CIRCLE('',#2287,4.86400000000037) ;
#829 = CIRCLE('',#2290,4.70000000000036) ;
#830 = CIRCLE('',#2292,1.00000000000008) ;
#831 = CIRCLE('',#2293,1.00000000000008) ;
#832 = CIRCLE('',#2295,1.00000000000008) ;
#833 = CIRCLE('',#2299,1.00000000000008) ;
#834 = CIRCLE('',#2302,1.00000000000008) ;
#835 = CIRCLE('',#2303,1.00000000000008) ;
#836 = CIRCLE('',#2305,1.00000000000008) ;
#837 = CIRCLE('',#2306,1.00000000000008) ;
#838 = CIRCLE('',#2308,1.00000000000008) ;
#839 = CIRCLE('',#2309,1.00000000000008) ;
#840 = CIRCLE('',#2311,1.00000000000008) ;
#841 = CIRCLE('',#2312,1.00000000000008) ;
#842 = CIRCLE('',#2314,1.00000000000008) ;
#843 = CIRCLE('',#2315,1.00000000000008) ;
#844 = CIRCLE('',#2317,1.00000000000008) ;
#845 = CIRCLE('',#2321,1.00000000000008) ;
#846 = CIRCLE('',#2324,1.00000000000008) ;
#847 = CIRCLE('',#2328,1.00000000000008) ;
#848 = CIRCLE('',#2331,1.00000000000008) ;
#849 = CIRCLE('',#2335,1.00000000000008) ;
#850 = CIRCLE('',#2338,1.00000000000008) ;
#851 = CIRCLE('',#2342,1.00000000000008) ;
#852 = CIRCLE('',#2345,1.00000000000008) ;
#853 = CIRCLE('',#2349,1.00000000000008) ;
#854 = CIRCLE('',#2352,5.79274121460045) ;
#855 = CIRCLE('',#2354,0.300000000000023) ;
#856 = CIRCLE('',#2355,6.07303514434047) ;
#857 = CIRCLE('',#2356,6.07303514434047) ;
#858 = CIRCLE('',#2358,4.70000000000036) ;
#859 = CIRCLE('',#2359,4.70000000000036) ;
#860 = CIRCLE('',#2361,6.50000000000051) ;
#861 = CIRCLE('',#2362,4.77941176471037) ;
#862 = CIRCLE('',#2363,4.77941176471037) ;
#863 = CIRCLE('',#2365,0.300000000000023) ;
#864 = CIRCLE('',#2368,6.85000000000052) ;
#865 = CIRCLE('',#2369,6.85000000000052) ;
#866 = CIRCLE('',#2371,6.00000000000046) ;
#867 = CIRCLE('',#2372,6.00000000000046) ;
#868 = CIRCLE('',#2374,2.50000000000019) ;
#869 = CIRCLE('',#2376,2.50000000000019) ;
#870 = CIRCLE('',#2378,2.20000000000017) ;
#871 = CIRCLE('',#2380,1.00000000000008) ;
#872 = CIRCLE('',#2381,1.3000000000001) ;
#873 = CIRCLE('',#2383,1.00000000000008) ;
#874 = CIRCLE('',#2385,4.25000000000032) ;
#875 = CIRCLE('',#2387,4.25000000000032) ;
#876 = CIRCLE('',#2389,4.28300000000033) ;
#877 = CIRCLE('',#2390,4.86400000000037) ;
#878 = CIRCLE('',#2392,4.28300000000033) ;
#879 = CIRCLE('',#2394,5.00000000000038) ;
#880 = CIRCLE('',#2396,5.00000000000038) ;
#881 = CIRCLE('',#2398,5.20000000000039) ;
#882 = CIRCLE('',#2404,0.300000000000023) ;
#883 = CIRCLE('',#2406,1.3000000000001) ;
#884 = CIRCLE('',#2407,1.3000000000001) ;
#885 = CIRCLE('',#2409,0.700000000000053) ;
#886 = CIRCLE('',#2411,0.300000000000023) ;
#887 = CIRCLE('',#2413,0.300000000000023) ;
#888 = CIRCLE('',#2415,0.850000000000065) ;
#889 = CIRCLE('',#2417,0.850000000000065) ;
#890 = CIRCLE('',#2419,3.55000000000027) ;
#891 = CIRCLE('',#2420,3.55000000000027) ;
#892 = CIRCLE('',#2422,4.25000000000032) ;
#893 = CIRCLE('',#2424,4.25000000000032) ;
#894 = CIRCLE('',#2426,3.00000000000023) ;
#895 = CIRCLE('',#2428,3.00000000000023) ;
#896 = CIRCLE('',#2430,0.300000000000023) ;
#897 = CIRCLE('',#2431,0.300000000000023) ;
#898 = CIRCLE('',#2436,2.00000000000015) ;
#899 = CIRCLE('',#2437,1.2500000000001) ;
#900 = CIRCLE('',#2439,2.05000000000016) ;
#901 = CIRCLE('',#2440,1.3000000000001) ;
#902 = CIRCLE('',#2442,1.3000000000001) ;
#903 = CIRCLE('',#2443,1.3000000000001) ;
#904 = CIRCLE('',#2444,4.00000013651843) ;
#905 = CIRCLE('',#2445,3.9999999789986) ;
#906 = CIRCLE('',#2446,1.29500935558696) ;
#907 = CIRCLE('',#2448,2.00000000000015) ;
#908 = CIRCLE('',#2449,2.00000000000015) ;
#909 = CIRCLE('',#2451,2.00499064449015) ;
#910 = CIRCLE('',#2452,4.0000000000003) ;
#911 = CIRCLE('',#2453,2.00499064449015) ;
#912 = CIRCLE('',#2455,2.05000000000016) ;
#913 = CIRCLE('',#2456,2.05000000000016) ;
#914 = CIRCLE('',#2458,2.04407360967015) ;
#915 = CIRCLE('',#2459,2.04407360967015) ;
#916 = CIRCLE('',#2460,4.75024664381333) ;
#917 = CIRCLE('',#2461,4.74999996695025) ;
#918 = CIRCLE('',#2463,1.2500000000001) ;
#919 = CIRCLE('',#2465,1.2559263903301) ;
#920 = CIRCLE('',#2467,4.75000000000036) ;
#921 = CIRCLE('',#2470,4.1) ;
#922 = CIRCLE('',#2471,4.1) ;
#923 = CIRCLE('',#2473,3.) ;
#924 = CIRCLE('',#2475,3.) ;
#925 = CIRCLE('',#2477,4.59619407771) ;
#926 = CIRCLE('',#2479,6.15142259969) ;
#927 = CIRCLE('',#2480,6.5) ;
#928 = CIRCLE('',#2482,5.7927412146) ;
#929 = CIRCLE('',#2484,0.3) ;
#930 = CIRCLE('',#2485,6.07303514434) ;
#931 = CIRCLE('',#2486,6.07303514434) ;
#932 = CIRCLE('',#2488,6.5) ;
#933 = CIRCLE('',#2489,4.77941176471) ;
#934 = CIRCLE('',#2490,4.77941176471) ;
#935 = CIRCLE('',#2492,0.3) ;
#936 = CIRCLE('',#2493,4.7) ;
#937 = CIRCLE('',#2494,4.7) ;
#938 = CIRCLE('',#2496,4.7) ;
#939 = CIRCLE('',#2497,4.7) ;
#940 = CIRCLE('',#2499,1.) ;
#941 = CIRCLE('',#2500,4.76165688318) ;
#942 = CIRCLE('',#2501,4.76165688318) ;
#943 = CIRCLE('',#2503,8.2) ;
#944 = CIRCLE('',#2504,8.2) ;
#945 = CIRCLE('',#2505,0.3) ;
#946 = CIRCLE('',#2506,7.9) ;
#947 = CIRCLE('',#2508,8.13834311682) ;
#948 = CIRCLE('',#2510,8.2) ;
#949 = CIRCLE('',#2512,1.) ;
#950 = CIRCLE('',#2514,6.15142259969) ;
#951 = CIRCLE('',#2516,6.35142259969) ;
#952 = CIRCLE('',#2518,0.2) ;
#953 = VERTEX_POINT('',#3286) ;
#954 = VERTEX_POINT('',#3288) ;
#955 = VERTEX_POINT('',#3292) ;
#956 = VERTEX_POINT('',#3296) ;
#957 = VERTEX_POINT('',#3300) ;
#958 = VERTEX_POINT('',#3304) ;
#959 = VERTEX_POINT('',#3308) ;
#960 = VERTEX_POINT('',#3310) ;
#961 = VERTEX_POINT('',#3312) ;
#962 = VERTEX_POINT('',#3316) ;
#963 = VERTEX_POINT('',#3317) ;
#964 = VERTEX_POINT('',#3320) ;
#965 = VERTEX_POINT('',#3324) ;
#966 = VERTEX_POINT('',#3326) ;
#967 = VERTEX_POINT('',#3330) ;
#968 = VERTEX_POINT('',#3332) ;
#969 = VERTEX_POINT('',#3336) ;
#970 = VERTEX_POINT('',#3337) ;
#971 = VERTEX_POINT('',#3342) ;
#972 = VERTEX_POINT('',#3344) ;
#973 = VERTEX_POINT('',#3350) ;
#974 = VERTEX_POINT('',#3354) ;
#975 = VERTEX_POINT('',#3359) ;
#976 = VERTEX_POINT('',#3360) ;
#977 = VERTEX_POINT('',#3365) ;
#978 = VERTEX_POINT('',#3371) ;
#979 = VERTEX_POINT('',#3373) ;
#980 = VERTEX_POINT('',#3377) ;
#981 = VERTEX_POINT('',#3380) ;
#982 = VERTEX_POINT('',#3384) ;
#983 = VERTEX_POINT('',#3388) ;
#984 = VERTEX_POINT('',#3392) ;
#985 = VERTEX_POINT('',#3396) ;
#986 = VERTEX_POINT('',#3399) ;
#987 = VERTEX_POINT('',#3403) ;
#988 = VERTEX_POINT('',#3407) ;
#989 = VERTEX_POINT('',#3408) ;
#990 = VERTEX_POINT('',#3410) ;
#991 = VERTEX_POINT('',#3412) ;
#992 = VERTEX_POINT('',#3414) ;
#993 = VERTEX_POINT('',#3416) ;
#994 = VERTEX_POINT('',#3420) ;
#995 = VERTEX_POINT('',#3421) ;
#996 = VERTEX_POINT('',#3423) ;
#997 = VERTEX_POINT('',#3425) ;
#998 = VERTEX_POINT('',#3427) ;
#999 = VERTEX_POINT('',#3429) ;
#1000 = VERTEX_POINT('',#3432) ;
#1001 = VERTEX_POINT('',#3437) ;
#1002 = VERTEX_POINT('',#3438) ;
#1003 = VERTEX_POINT('',#3440) ;
#1004 = VERTEX_POINT('',#3442) ;
#1005 = VERTEX_POINT('',#3446) ;
#1006 = VERTEX_POINT('',#3448) ;
#1007 = VERTEX_POINT('',#3452) ;
#1008 = VERTEX_POINT('',#3456) ;
#1009 = VERTEX_POINT('',#3464) ;
#1010 = VERTEX_POINT('',#3465) ;
#1011 = VERTEX_POINT('',#3467) ;
#1012 = VERTEX_POINT('',#3469) ;
#1013 = VERTEX_POINT('',#3474) ;
#1014 = VERTEX_POINT('',#3475) ;
#1015 = VERTEX_POINT('',#3477) ;
#1016 = VERTEX_POINT('',#3479) ;
#1017 = VERTEX_POINT('',#3484) ;
#1018 = VERTEX_POINT('',#3485) ;
#1019 = VERTEX_POINT('',#3487) ;
#1020 = VERTEX_POINT('',#3489) ;
#1021 = VERTEX_POINT('',#3494) ;
#1022 = VERTEX_POINT('',#3495) ;
#1023 = VERTEX_POINT('',#3497) ;
#1024 = VERTEX_POINT('',#3499) ;
#1025 = VERTEX_POINT('',#3503) ;
#1026 = VERTEX_POINT('',#3504) ;
#1027 = VERTEX_POINT('',#3506) ;
#1028 = VERTEX_POINT('',#3508) ;
#1029 = VERTEX_POINT('',#3512) ;
#1030 = VERTEX_POINT('',#3514) ;
#1031 = VERTEX_POINT('',#3518) ;
#1032 = VERTEX_POINT('',#3522) ;
#1033 = VERTEX_POINT('',#3529) ;
#1034 = VERTEX_POINT('',#3531) ;
#1035 = VERTEX_POINT('',#3535) ;
#1036 = VERTEX_POINT('',#3539) ;
#1037 = VERTEX_POINT('',#3546) ;
#1038 = VERTEX_POINT('',#3548) ;
#1039 = VERTEX_POINT('',#3552) ;
#1040 = VERTEX_POINT('',#3556) ;
#1041 = VERTEX_POINT('',#3563) ;
#1042 = VERTEX_POINT('',#3565) ;
#1043 = VERTEX_POINT('',#3569) ;
#1044 = VERTEX_POINT('',#3573) ;
#1045 = VERTEX_POINT('',#3580) ;
#1046 = VERTEX_POINT('',#3582) ;
#1047 = VERTEX_POINT('',#3586) ;
#1048 = VERTEX_POINT('',#3590) ;
#1049 = VERTEX_POINT('',#3597) ;
#1050 = VERTEX_POINT('',#3600) ;
#1051 = VERTEX_POINT('',#3602) ;
#1052 = VERTEX_POINT('',#3606) ;
#1053 = VERTEX_POINT('',#3607) ;
#1054 = VERTEX_POINT('',#3612) ;
#1055 = VERTEX_POINT('',#3614) ;
#1056 = VERTEX_POINT('',#3621) ;
#1057 = VERTEX_POINT('',#3623) ;
#1058 = VERTEX_POINT('',#3627) ;
#1059 = VERTEX_POINT('',#3629) ;
#1060 = VERTEX_POINT('',#3633) ;
#1061 = VERTEX_POINT('',#3637) ;
#1062 = VERTEX_POINT('',#3641) ;
#1063 = VERTEX_POINT('',#3645) ;
#1064 = VERTEX_POINT('',#3647) ;
#1065 = VERTEX_POINT('',#3651) ;
#1066 = VERTEX_POINT('',#3655) ;
#1067 = VERTEX_POINT('',#3659) ;
#1068 = VERTEX_POINT('',#3663) ;
#1069 = VERTEX_POINT('',#3665) ;
#1070 = VERTEX_POINT('',#3669) ;
#1071 = VERTEX_POINT('',#3673) ;
#1072 = VERTEX_POINT('',#3677) ;
#1073 = VERTEX_POINT('',#3681) ;
#1074 = VERTEX_POINT('',#3689) ;
#1075 = VERTEX_POINT('',#3691) ;
#1076 = VERTEX_POINT('',#3732) ;
#1077 = VERTEX_POINT('',#3734) ;
#1078 = VERTEX_POINT('',#3738) ;
#1079 = VERTEX_POINT('',#3741) ;
#1080 = VERTEX_POINT('',#3745) ;
#1081 = VERTEX_POINT('',#3749) ;
#1082 = VERTEX_POINT('',#3752) ;
#1083 = VERTEX_POINT('',#3756) ;
#1084 = VERTEX_POINT('',#3758) ;
#1085 = VERTEX_POINT('',#3762) ;
#1086 = VERTEX_POINT('',#3765) ;
#1087 = VERTEX_POINT('',#3769) ;
#1088 = VERTEX_POINT('',#3772) ;
#1089 = VERTEX_POINT('',#3776) ;
#1090 = VERTEX_POINT('',#3778) ;
#1091 = VERTEX_POINT('',#3782) ;
#1092 = VERTEX_POINT('',#3783) ;
#1093 = VERTEX_POINT('',#3829) ;
#1094 = VERTEX_POINT('',#3830) ;
#1095 = VERTEX_POINT('',#3881) ;
#1096 = VERTEX_POINT('',#3883) ;
#1097 = VERTEX_POINT('',#3886) ;
#1098 = VERTEX_POINT('',#3888) ;
#1099 = VERTEX_POINT('',#3891) ;
#1100 = VERTEX_POINT('',#3892) ;
#1101 = VERTEX_POINT('',#3941) ;
#1102 = VERTEX_POINT('',#3942) ;
#1103 = VERTEX_POINT('',#4074) ;
#1104 = VERTEX_POINT('',#4075) ;
#1105 = VERTEX_POINT('',#4080) ;
#1106 = VERTEX_POINT('',#4081) ;
#1107 = VERTEX_POINT('',#4086) ;
#1108 = VERTEX_POINT('',#4088) ;
#1109 = VERTEX_POINT('',#4092) ;
#1110 = VERTEX_POINT('',#4093) ;
#1111 = VERTEX_POINT('',#4190) ;
#1112 = VERTEX_POINT('',#4194) ;
#1113 = VERTEX_POINT('',#4201) ;
#1114 = VERTEX_POINT('',#4203) ;
#1115 = VERTEX_POINT('',#4207) ;
#1116 = VERTEX_POINT('',#4211) ;
#1117 = VERTEX_POINT('',#4215) ;
#1118 = VERTEX_POINT('',#4219) ;
#1119 = VERTEX_POINT('',#4223) ;
#1120 = VERTEX_POINT('',#4226) ;
#1121 = VERTEX_POINT('',#4228) ;
#1122 = VERTEX_POINT('',#4232) ;
#1123 = VERTEX_POINT('',#4234) ;
#1124 = VERTEX_POINT('',#4238) ;
#1125 = VERTEX_POINT('',#4240) ;
#1126 = VERTEX_POINT('',#4244) ;
#1127 = VERTEX_POINT('',#4246) ;
#1128 = VERTEX_POINT('',#4250) ;
#1129 = VERTEX_POINT('',#4252) ;
#1130 = VERTEX_POINT('',#4256) ;
#1131 = VERTEX_POINT('',#4257) ;
#1132 = VERTEX_POINT('',#4260) ;
#1133 = VERTEX_POINT('',#4264) ;
#1134 = VERTEX_POINT('',#4268) ;
#1135 = VERTEX_POINT('',#4274) ;
#1136 = VERTEX_POINT('',#4278) ;
#1137 = EDGE_CURVE('',#953,#953,#784,.T.) ;
#1138 = EDGE_CURVE('',#953,#954,#785,.T.) ;
#1139 = EDGE_CURVE('',#954,#954,#786,.T.) ;
#1140 = EDGE_CURVE('',#955,#955,#787,.T.) ;
#1141 = EDGE_CURVE('',#955,#953,#223,.T.) ;
#1142 = EDGE_CURVE('',#956,#956,#788,.T.) ;
#1143 = EDGE_CURVE('',#956,#955,#224,.T.) ;
#1144 = EDGE_CURVE('',#956,#957,#225,.T.) ;
#1145 = EDGE_CURVE('',#957,#957,#789,.F.) ;
#1146 = EDGE_CURVE('',#958,#958,#790,.T.) ;
#1147 = EDGE_CURVE('',#958,#957,#791,.T.) ;
#1148 = EDGE_CURVE('',#959,#959,#792,.T.) ;
#1149 = EDGE_CURVE('',#959,#960,#793,.T.) ;
#1150 = EDGE_CURVE('',#960,#961,#794,.T.) ;
#1151 = EDGE_CURVE('',#961,#960,#795,.T.) ;
#1152 = EDGE_CURVE('',#962,#963,#796,.T.) ;
#1153 = EDGE_CURVE('',#963,#962,#797,.T.) ;
#1154 = EDGE_CURVE('',#963,#964,#798,.T.) ;
#1155 = EDGE_CURVE('',#964,#964,#799,.T.) ;
#1156 = EDGE_CURVE('',#961,#965,#800,.T.) ;
#1157 = EDGE_CURVE('',#966,#965,#801,.F.) ;
#1158 = EDGE_CURVE('',#965,#966,#802,.F.) ;
#1159 = EDGE_CURVE('',#966,#967,#803,.T.) ;
#1160 = EDGE_CURVE('',#968,#967,#804,.F.) ;
#1161 = EDGE_CURVE('',#967,#968,#805,.F.) ;
#1162 = EDGE_CURVE('',#969,#970,#806,.F.) ;
#1163 = EDGE_CURVE('',#970,#962,#807,.T.) ;
#1164 = EDGE_CURVE('',#970,#969,#808,.F.) ;
#1165 = EDGE_CURVE('',#968,#971,#226,.T.) ;
#1166 = EDGE_CURVE('',#972,#971,#809,.F.) ;
#1167 = EDGE_CURVE('',#971,#972,#810,.F.) ;
#1168 = EDGE_CURVE('',#972,#969,#811,.T.) ;
#1169 = EDGE_CURVE('',#954,#973,#227,.T.) ;
#1170 = EDGE_CURVE('',#973,#973,#812,.T.) ;
#1171 = EDGE_CURVE('',#974,#974,#813,.T.) ;
#1172 = EDGE_CURVE('',#973,#974,#814,.T.) ;
#1173 = EDGE_CURVE('',#975,#976,#815,.T.) ;
#1174 = EDGE_CURVE('',#976,#975,#816,.T.) ;
#1175 = EDGE_CURVE('',#976,#958,#228,.T.) ;
#1176 = EDGE_CURVE('',#977,#977,#817,.T.) ;
#1177 = EDGE_CURVE('',#977,#975,#818,.T.) ;
#1178 = EDGE_CURVE('',#978,#978,#819,.T.) ;
#1179 = EDGE_CURVE('',#978,#979,#229,.T.) ;
#1180 = EDGE_CURVE('',#979,#979,#820,.T.) ;
#1181 = EDGE_CURVE('',#980,#980,#821,.T.) ;
#1182 = EDGE_CURVE('',#981,#981,#822,.T.) ;
#1183 = EDGE_CURVE('',#981,#978,#230,.T.) ;
#1184 = EDGE_CURVE('',#980,#982,#231,.T.) ;
#1185 = EDGE_CURVE('',#982,#982,#823,.T.) ;
#1186 = EDGE_CURVE('',#981,#983,#232,.T.) ;
#1187 = EDGE_CURVE('',#983,#983,#824,.F.) ;
#1188 = EDGE_CURVE('',#982,#984,#233,.T.) ;
#1189 = EDGE_CURVE('',#984,#984,#825,.T.) ;
#1190 = EDGE_CURVE('',#985,#985,#826,.T.) ;
#1191 = EDGE_CURVE('',#984,#986,#234,.T.) ;
#1192 = EDGE_CURVE('',#986,#986,#827,.T.) ;
#1193 = EDGE_CURVE('',#987,#987,#828,.T.) ;
#1194 = EDGE_CURVE('',#987,#985,#235,.T.) ;
#1195 = EDGE_CURVE('',#988,#989,#236,.T.) ;
#1196 = EDGE_CURVE('',#989,#990,#237,.T.) ;
#1197 = EDGE_CURVE('',#990,#991,#238,.T.) ;
#1198 = EDGE_CURVE('',#991,#992,#239,.T.) ;
#1199 = EDGE_CURVE('',#992,#993,#240,.T.) ;
#1200 = EDGE_CURVE('',#993,#988,#241,.T.) ;
#1201 = EDGE_CURVE('',#994,#995,#242,.T.) ;
#1202 = EDGE_CURVE('',#996,#994,#243,.T.) ;
#1203 = EDGE_CURVE('',#997,#996,#244,.T.) ;
#1204 = EDGE_CURVE('',#998,#997,#245,.T.) ;
#1205 = EDGE_CURVE('',#999,#998,#246,.T.) ;
#1206 = EDGE_CURVE('',#995,#999,#247,.T.) ;
#1207 = EDGE_CURVE('',#1000,#1000,#829,.T.) ;
#1208 = EDGE_CURVE('',#992,#994,#248,.T.) ;
#1209 = EDGE_CURVE('',#991,#996,#249,.T.) ;
#1210 = EDGE_CURVE('',#1001,#1002,#830,.F.) ;
#1211 = EDGE_CURVE('',#1003,#1001,#250,.F.) ;
#1212 = EDGE_CURVE('',#1004,#1003,#831,.F.) ;
#1213 = EDGE_CURVE('',#1002,#1004,#251,.F.) ;
#1214 = EDGE_CURVE('',#1004,#1005,#252,.F.) ;
#1215 = EDGE_CURVE('',#1003,#1006,#253,.F.) ;
#1216 = EDGE_CURVE('',#1005,#1006,#832,.T.) ;
#1217 = EDGE_CURVE('',#1002,#1007,#254,.T.) ;
#1218 = EDGE_CURVE('',#1007,#1005,#255,.F.) ;
#1219 = EDGE_CURVE('',#1001,#1008,#256,.T.) ;
#1220 = EDGE_CURVE('',#1006,#1008,#257,.F.) ;
#1221 = EDGE_CURVE('',#1008,#1007,#833,.T.) ;
#1222 = EDGE_CURVE('',#990,#997,#258,.T.) ;
#1223 = EDGE_CURVE('',#1009,#1010,#259,.F.) ;
#1224 = EDGE_CURVE('',#1011,#1009,#834,.F.) ;
#1225 = EDGE_CURVE('',#1012,#1011,#260,.F.) ;
#1226 = EDGE_CURVE('',#1010,#1012,#835,.F.) ;
#1227 = EDGE_CURVE('',#993,#995,#261,.T.) ;
#1228 = EDGE_CURVE('',#1013,#1014,#262,.F.) ;
#1229 = EDGE_CURVE('',#1015,#1013,#836,.F.) ;
#1230 = EDGE_CURVE('',#1016,#1015,#263,.F.) ;
#1231 = EDGE_CURVE('',#1014,#1016,#837,.F.) ;
#1232 = EDGE_CURVE('',#989,#998,#264,.T.) ;
#1233 = EDGE_CURVE('',#1017,#1018,#265,.F.) ;
#1234 = EDGE_CURVE('',#1019,#1017,#838,.F.) ;
#1235 = EDGE_CURVE('',#1020,#1019,#266,.F.) ;
#1236 = EDGE_CURVE('',#1018,#1020,#839,.F.) ;
#1237 = EDGE_CURVE('',#988,#999,#267,.T.) ;
#1238 = EDGE_CURVE('',#1021,#1022,#268,.F.) ;
#1239 = EDGE_CURVE('',#1023,#1021,#840,.F.) ;
#1240 = EDGE_CURVE('',#1024,#1023,#269,.F.) ;
#1241 = EDGE_CURVE('',#1022,#1024,#841,.F.) ;
#1242 = EDGE_CURVE('',#1025,#1026,#270,.F.) ;
#1243 = EDGE_CURVE('',#1027,#1025,#842,.F.) ;
#1244 = EDGE_CURVE('',#1028,#1027,#271,.F.) ;
#1245 = EDGE_CURVE('',#1026,#1028,#843,.F.) ;
#1246 = EDGE_CURVE('',#1027,#1029,#272,.F.) ;
#1247 = EDGE_CURVE('',#1025,#1030,#273,.F.) ;
#1248 = EDGE_CURVE('',#1029,#1030,#844,.T.) ;
#1249 = EDGE_CURVE('',#1028,#1031,#274,.T.) ;
#1250 = EDGE_CURVE('',#1031,#1029,#275,.F.) ;
#1251 = EDGE_CURVE('',#1026,#1032,#276,.T.) ;
#1252 = EDGE_CURVE('',#1030,#1032,#277,.F.) ;
#1253 = EDGE_CURVE('',#1032,#1031,#845,.T.) ;
#1254 = EDGE_CURVE('',#1015,#1033,#278,.F.) ;
#1255 = EDGE_CURVE('',#1013,#1034,#279,.F.) ;
#1256 = EDGE_CURVE('',#1033,#1034,#846,.T.) ;
#1257 = EDGE_CURVE('',#1016,#1035,#280,.T.) ;
#1258 = EDGE_CURVE('',#1035,#1033,#281,.F.) ;
#1259 = EDGE_CURVE('',#1014,#1036,#282,.T.) ;
#1260 = EDGE_CURVE('',#1034,#1036,#283,.F.) ;
#1261 = EDGE_CURVE('',#1036,#1035,#847,.T.) ;
#1262 = EDGE_CURVE('',#1019,#1037,#284,.F.) ;
#1263 = EDGE_CURVE('',#1017,#1038,#285,.F.) ;
#1264 = EDGE_CURVE('',#1037,#1038,#848,.T.) ;
#1265 = EDGE_CURVE('',#1020,#1039,#286,.T.) ;
#1266 = EDGE_CURVE('',#1039,#1037,#287,.F.) ;
#1267 = EDGE_CURVE('',#1018,#1040,#288,.T.) ;
#1268 = EDGE_CURVE('',#1038,#1040,#289,.F.) ;
#1269 = EDGE_CURVE('',#1040,#1039,#849,.T.) ;
#1270 = EDGE_CURVE('',#1011,#1041,#290,.F.) ;
#1271 = EDGE_CURVE('',#1009,#1042,#291,.F.) ;
#1272 = EDGE_CURVE('',#1041,#1042,#850,.T.) ;
#1273 = EDGE_CURVE('',#1012,#1043,#292,.T.) ;
#1274 = EDGE_CURVE('',#1043,#1041,#293,.F.) ;
#1275 = EDGE_CURVE('',#1010,#1044,#294,.T.) ;
#1276 = EDGE_CURVE('',#1042,#1044,#295,.F.) ;
#1277 = EDGE_CURVE('',#1044,#1043,#851,.T.) ;
#1278 = EDGE_CURVE('',#1023,#1045,#296,.F.) ;
#1279 = EDGE_CURVE('',#1021,#1046,#297,.F.) ;
#1280 = EDGE_CURVE('',#1045,#1046,#852,.T.) ;
#1281 = EDGE_CURVE('',#1024,#1047,#298,.T.) ;
#1282 = EDGE_CURVE('',#1047,#1045,#299,.F.) ;
#1283 = EDGE_CURVE('',#1022,#1048,#300,.T.) ;
#1284 = EDGE_CURVE('',#1046,#1048,#301,.F.) ;
#1285 = EDGE_CURVE('',#1048,#1047,#853,.T.) ;
#1286 = EDGE_CURVE('',#1049,#1049,#854,.T.) ;
#1287 = EDGE_CURVE('',#1049,#1050,#855,.T.) ;
#1288 = EDGE_CURVE('',#1050,#1051,#856,.T.) ;
#1289 = EDGE_CURVE('',#1051,#1050,#857,.T.) ;
#1290 = EDGE_CURVE('',#1052,#1053,#858,.F.) ;
#1291 = EDGE_CURVE('',#1053,#1000,#302,.T.) ;
#1292 = EDGE_CURVE('',#1053,#1052,#859,.F.) ;
#1293 = EDGE_CURVE('',#1051,#1054,#860,.T.) ;
#1294 = EDGE_CURVE('',#1055,#1054,#861,.F.) ;
#1295 = EDGE_CURVE('',#1054,#1055,#862,.F.) ;
#1296 = EDGE_CURVE('',#1055,#1052,#863,.T.) ;
#1297 = EDGE_CURVE('',#1056,#1056,#864,.T.) ;
#1298 = EDGE_CURVE('',#1056,#1057,#303,.T.) ;
#1299 = EDGE_CURVE('',#1057,#1057,#865,.T.) ;
#1300 = EDGE_CURVE('',#1058,#1058,#866,.T.) ;
#1301 = EDGE_CURVE('',#1058,#1059,#304,.T.) ;
#1302 = EDGE_CURVE('',#1059,#1059,#867,.T.) ;
#1303 = EDGE_CURVE('',#1058,#1060,#305,.T.) ;
#1304 = EDGE_CURVE('',#1060,#1060,#868,.F.) ;
#1305 = EDGE_CURVE('',#1061,#1061,#869,.T.) ;
#1306 = EDGE_CURVE('',#1061,#1060,#306,.T.) ;
#1307 = EDGE_CURVE('',#1061,#1062,#307,.T.) ;
#1308 = EDGE_CURVE('',#1062,#1062,#870,.F.) ;
#1309 = EDGE_CURVE('',#1063,#1063,#871,.T.) ;
#1310 = EDGE_CURVE('',#1063,#1064,#308,.T.) ;
#1311 = EDGE_CURVE('',#1064,#1064,#872,.T.) ;
#1312 = EDGE_CURVE('',#1065,#1065,#873,.T.) ;
#1313 = EDGE_CURVE('',#1065,#1063,#309,.T.) ;
#1314 = EDGE_CURVE('',#1065,#1066,#310,.T.) ;
#1315 = EDGE_CURVE('',#1066,#1066,#874,.F.) ;
#1316 = EDGE_CURVE('',#1067,#1067,#875,.T.) ;
#1317 = EDGE_CURVE('',#1067,#1066,#311,.T.) ;
#1318 = EDGE_CURVE('',#1068,#1068,#876,.T.) ;
#1319 = EDGE_CURVE('',#1068,#1069,#312,.T.) ;
#1320 = EDGE_CURVE('',#1069,#1069,#877,.T.) ;
#1321 = EDGE_CURVE('',#1070,#1070,#878,.T.) ;
#1322 = EDGE_CURVE('',#1070,#1068,#313,.T.) ;
#1323 = EDGE_CURVE('',#1070,#1071,#314,.T.) ;
#1324 = EDGE_CURVE('',#1071,#1071,#879,.F.) ;
#1325 = EDGE_CURVE('',#1072,#1072,#880,.T.) ;
#1326 = EDGE_CURVE('',#1072,#1071,#315,.T.) ;
#1327 = EDGE_CURVE('',#1072,#1073,#316,.T.) ;
#1328 = EDGE_CURVE('',#1073,#1073,#881,.F.) ;
#1329 = EDGE_CURVE('',#1074,#1074,#882,.T.) ;
#1330 = EDGE_CURVE('',#1074,#1075,#317,.T.) ;
#1331 = EDGE_CURVE('',#1075,#1075,#59,.T.) ;
#1332 = EDGE_CURVE('',#1076,#1076,#883,.T.) ;
#1333 = EDGE_CURVE('',#1076,#1077,#318,.T.) ;
#1334 = EDGE_CURVE('',#1077,#1077,#884,.T.) ;
#1335 = EDGE_CURVE('',#1078,#1078,#885,.T.) ;
#1336 = EDGE_CURVE('',#1079,#1079,#886,.F.) ;
#1337 = EDGE_CURVE('',#1079,#1078,#319,.T.) ;
#1338 = EDGE_CURVE('',#1079,#1080,#320,.T.) ;
#1339 = EDGE_CURVE('',#1080,#1080,#887,.T.) ;
#1340 = EDGE_CURVE('',#1081,#1081,#888,.T.) ;
#1341 = EDGE_CURVE('',#1081,#1082,#321,.T.) ;
#1342 = EDGE_CURVE('',#1082,#1082,#889,.T.) ;
#1343 = EDGE_CURVE('',#1083,#1083,#890,.T.) ;
#1344 = EDGE_CURVE('',#1083,#1084,#322,.T.) ;
#1345 = EDGE_CURVE('',#1084,#1084,#891,.T.) ;
#1346 = EDGE_CURVE('',#1085,#1085,#892,.T.) ;
#1347 = EDGE_CURVE('',#1085,#1086,#323,.T.) ;
#1348 = EDGE_CURVE('',#1086,#1086,#893,.T.) ;
#1349 = EDGE_CURVE('',#1087,#1087,#894,.T.) ;
#1350 = EDGE_CURVE('',#1087,#1088,#324,.T.) ;
#1351 = EDGE_CURVE('',#1088,#1088,#895,.T.) ;
#1352 = EDGE_CURVE('',#1089,#1089,#896,.T.) ;
#1353 = EDGE_CURVE('',#1090,#1090,#897,.T.) ;
#1354 = EDGE_CURVE('',#1083,#1082,#325,.T.) ;
#1355 = EDGE_CURVE('',#1091,#1092,#60,.T.) ;
#1356 = EDGE_CURVE('',#1092,#1091,#61,.T.) ;
#1357 = EDGE_CURVE('',#1093,#1094,#62,.T.) ;
#1358 = EDGE_CURVE('',#1094,#1093,#63,.T.) ;
#1359 = EDGE_CURVE('',#1089,#1092,#326,.T.) ;
#1360 = EDGE_CURVE('',#1090,#1094,#327,.T.) ;
#1361 = EDGE_CURVE('',#1095,#1095,#898,.T.) ;
#1362 = EDGE_CURVE('',#1096,#1096,#899,.T.) ;
#1363 = EDGE_CURVE('',#1097,#1097,#900,.T.) ;
#1364 = EDGE_CURVE('',#1098,#1098,#901,.T.) ;
#1365 = EDGE_CURVE('',#1099,#1100,#902,.F.) ;
#1366 = EDGE_CURVE('',#1100,#1099,#903,.F.) ;
#1367 = EDGE_CURVE('',#1099,#1098,#328,.T.) ;
#1368 = EDGE_CURVE('',#1101,#1102,#64,.T.) ;
#1369 = EDGE_CURVE('',#1102,#1099,#904,.F.) ;
#1370 = EDGE_CURVE('',#1101,#1100,#905,.F.) ;
#1371 = EDGE_CURVE('',#1102,#1101,#906,.T.) ;
#1372 = EDGE_CURVE('',#1103,#1104,#907,.F.) ;
#1373 = EDGE_CURVE('',#1104,#1095,#329,.T.) ;
#1374 = EDGE_CURVE('',#1104,#1103,#908,.F.) ;
#1375 = EDGE_CURVE('',#1105,#1106,#909,.F.) ;
#1376 = EDGE_CURVE('',#1106,#1103,#910,.T.) ;
#1377 = EDGE_CURVE('',#1106,#1105,#911,.F.) ;
#1378 = EDGE_CURVE('',#1097,#1107,#330,.T.) ;
#1379 = EDGE_CURVE('',#1107,#1108,#912,.T.) ;
#1380 = EDGE_CURVE('',#1108,#1107,#913,.T.) ;
#1381 = EDGE_CURVE('',#1109,#1110,#914,.T.) ;
#1382 = EDGE_CURVE('',#1110,#1109,#915,.T.) ;
#1383 = EDGE_CURVE('',#1110,#1105,#331,.T.) ;
#1384 = EDGE_CURVE('',#1107,#1110,#916,.F.) ;
#1385 = EDGE_CURVE('',#1108,#1109,#917,.F.) ;
#1386 = EDGE_CURVE('',#1096,#1111,#332,.T.) ;
#1387 = EDGE_CURVE('',#1111,#1111,#918,.T.) ;
#1388 = EDGE_CURVE('',#1112,#1112,#919,.T.) ;
#1389 = EDGE_CURVE('',#1112,#1102,#333,.T.) ;
#1390 = EDGE_CURVE('',#1112,#1111,#920,.T.) ;
#1391 = EDGE_CURVE('',#1113,#1113,#921,.T.) ;
#1392 = EDGE_CURVE('',#1113,#1114,#334,.T.) ;
#1393 = EDGE_CURVE('',#1114,#1114,#922,.T.) ;
#1394 = EDGE_CURVE('',#1115,#1115,#923,.T.) ;
#1395 = EDGE_CURVE('',#1115,#1113,#335,.T.) ;
#1396 = EDGE_CURVE('',#1116,#1116,#924,.T.) ;
#1397 = EDGE_CURVE('',#1116,#1115,#336,.T.) ;
#1398 = EDGE_CURVE('',#1116,#1117,#337,.T.) ;
#1399 = EDGE_CURVE('',#1117,#1117,#925,.F.) ;
#1400 = EDGE_CURVE('',#1118,#1118,#926,.T.) ;
#1401 = EDGE_CURVE('',#1118,#1117,#927,.T.) ;
#1402 = EDGE_CURVE('',#1119,#1119,#928,.T.) ;
#1403 = EDGE_CURVE('',#1119,#1120,#929,.T.) ;
#1404 = EDGE_CURVE('',#1120,#1121,#930,.T.) ;
#1405 = EDGE_CURVE('',#1121,#1120,#931,.T.) ;
#1406 = EDGE_CURVE('',#1121,#1122,#932,.T.) ;
#1407 = EDGE_CURVE('',#1123,#1122,#933,.F.) ;
#1408 = EDGE_CURVE('',#1122,#1123,#934,.F.) ;
#1409 = EDGE_CURVE('',#1123,#1124,#935,.T.) ;
#1410 = EDGE_CURVE('',#1125,#1124,#936,.F.) ;
#1411 = EDGE_CURVE('',#1124,#1125,#937,.F.) ;
#1412 = EDGE_CURVE('',#1125,#1126,#338,.T.) ;
#1413 = EDGE_CURVE('',#1127,#1126,#938,.F.) ;
#1414 = EDGE_CURVE('',#1126,#1127,#939,.F.) ;
#1415 = EDGE_CURVE('',#1127,#1128,#940,.T.) ;
#1416 = EDGE_CURVE('',#1129,#1128,#941,.F.) ;
#1417 = EDGE_CURVE('',#1128,#1129,#942,.F.) ;
#1418 = EDGE_CURVE('',#1130,#1131,#943,.T.) ;
#1419 = EDGE_CURVE('',#1131,#1130,#944,.T.) ;
#1420 = EDGE_CURVE('',#1131,#1132,#945,.T.) ;
#1421 = EDGE_CURVE('',#1132,#1132,#946,.T.) ;
#1422 = EDGE_CURVE('',#1133,#1133,#947,.F.) ;
#1423 = EDGE_CURVE('',#1133,#1129,#339,.T.) ;
#1424 = EDGE_CURVE('',#1134,#1134,#948,.T.) ;
#1425 = EDGE_CURVE('',#1134,#1130,#340,.T.) ;
#1426 = EDGE_CURVE('',#1134,#1133,#949,.T.) ;
#1427 = EDGE_CURVE('',#1135,#1135,#950,.T.) ;
#1428 = EDGE_CURVE('',#1135,#1118,#341,.T.) ;
#1429 = EDGE_CURVE('',#1136,#1136,#951,.T.) ;
#1430 = EDGE_CURVE('',#1136,#1135,#952,.T.) ;
#1431 = ORIENTED_EDGE('',*,*,#1137,.F.) ;
#1432 = ORIENTED_EDGE('',*,*,#1138,.T.) ;
#1433 = ORIENTED_EDGE('',*,*,#1139,.T.) ;
#1434 = ORIENTED_EDGE('',*,*,#1138,.F.) ;
#1435 = ORIENTED_EDGE('',*,*,#1140,.F.) ;
#1436 = ORIENTED_EDGE('',*,*,#1141,.T.) ;
#1437 = ORIENTED_EDGE('',*,*,#1137,.T.) ;
#1438 = ORIENTED_EDGE('',*,*,#1141,.F.) ;
#1439 = ORIENTED_EDGE('',*,*,#1142,.F.) ;
#1440 = ORIENTED_EDGE('',*,*,#1143,.T.) ;
#1441 = ORIENTED_EDGE('',*,*,#1140,.T.) ;
#1442 = ORIENTED_EDGE('',*,*,#1143,.F.) ;
#1443 = ORIENTED_EDGE('',*,*,#1142,.T.) ;
#1444 = ORIENTED_EDGE('',*,*,#1144,.T.) ;
#1445 = ORIENTED_EDGE('',*,*,#1145,.F.) ;
#1446 = ORIENTED_EDGE('',*,*,#1144,.F.) ;
#1447 = ORIENTED_EDGE('',*,*,#1146,.F.) ;
#1448 = ORIENTED_EDGE('',*,*,#1147,.T.) ;
#1449 = ORIENTED_EDGE('',*,*,#1145,.T.) ;
#1450 = ORIENTED_EDGE('',*,*,#1147,.F.) ;
#1451 = ORIENTED_EDGE('',*,*,#1148,.F.) ;
#1452 = ORIENTED_EDGE('',*,*,#1149,.T.) ;
#1453 = ORIENTED_EDGE('',*,*,#1150,.T.) ;
#1454 = ORIENTED_EDGE('',*,*,#1151,.T.) ;
#1455 = ORIENTED_EDGE('',*,*,#1149,.F.) ;
#1456 = ORIENTED_EDGE('',*,*,#1152,.F.) ;
#1457 = ORIENTED_EDGE('',*,*,#1153,.F.) ;
#1458 = ORIENTED_EDGE('',*,*,#1154,.T.) ;
#1459 = ORIENTED_EDGE('',*,*,#1155,.T.) ;
#1460 = ORIENTED_EDGE('',*,*,#1154,.F.) ;
#1461 = ORIENTED_EDGE('',*,*,#1151,.F.) ;
#1462 = ORIENTED_EDGE('',*,*,#1156,.T.) ;
#1463 = ORIENTED_EDGE('',*,*,#1157,.F.) ;
#1464 = ORIENTED_EDGE('',*,*,#1158,.F.) ;
#1465 = ORIENTED_EDGE('',*,*,#1156,.F.) ;
#1466 = ORIENTED_EDGE('',*,*,#1150,.F.) ;
#1467 = ORIENTED_EDGE('',*,*,#1157,.T.) ;
#1468 = ORIENTED_EDGE('',*,*,#1158,.T.) ;
#1469 = ORIENTED_EDGE('',*,*,#1159,.T.) ;
#1470 = ORIENTED_EDGE('',*,*,#1160,.F.) ;
#1471 = ORIENTED_EDGE('',*,*,#1161,.F.) ;
#1472 = ORIENTED_EDGE('',*,*,#1159,.F.) ;
#1473 = ORIENTED_EDGE('',*,*,#1162,.T.) ;
#1474 = ORIENTED_EDGE('',*,*,#1163,.T.) ;
#1475 = ORIENTED_EDGE('',*,*,#1152,.T.) ;
#1476 = ORIENTED_EDGE('',*,*,#1153,.T.) ;
#1477 = ORIENTED_EDGE('',*,*,#1163,.F.) ;
#1478 = ORIENTED_EDGE('',*,*,#1164,.T.) ;
#1479 = ORIENTED_EDGE('',*,*,#1160,.T.) ;
#1480 = ORIENTED_EDGE('',*,*,#1161,.T.) ;
#1481 = ORIENTED_EDGE('',*,*,#1165,.T.) ;
#1482 = ORIENTED_EDGE('',*,*,#1166,.F.) ;
#1483 = ORIENTED_EDGE('',*,*,#1167,.F.) ;
#1484 = ORIENTED_EDGE('',*,*,#1165,.F.) ;
#1485 = ORIENTED_EDGE('',*,*,#1166,.T.) ;
#1486 = ORIENTED_EDGE('',*,*,#1167,.T.) ;
#1487 = ORIENTED_EDGE('',*,*,#1168,.T.) ;
#1488 = ORIENTED_EDGE('',*,*,#1164,.F.) ;
#1489 = ORIENTED_EDGE('',*,*,#1162,.F.) ;
#1490 = ORIENTED_EDGE('',*,*,#1168,.F.) ;
#1491 = ORIENTED_EDGE('',*,*,#1139,.F.) ;
#1492 = ORIENTED_EDGE('',*,*,#1169,.T.) ;
#1493 = ORIENTED_EDGE('',*,*,#1170,.T.) ;
#1494 = ORIENTED_EDGE('',*,*,#1169,.F.) ;
#1495 = ORIENTED_EDGE('',*,*,#1148,.T.) ;
#1496 = ORIENTED_EDGE('',*,*,#1171,.F.) ;
#1497 = ORIENTED_EDGE('',*,*,#1170,.F.) ;
#1498 = ORIENTED_EDGE('',*,*,#1172,.T.) ;
#1499 = ORIENTED_EDGE('',*,*,#1171,.T.) ;
#1500 = ORIENTED_EDGE('',*,*,#1172,.F.) ;
#1501 = ORIENTED_EDGE('',*,*,#1173,.F.) ;
#1502 = ORIENTED_EDGE('',*,*,#1174,.F.) ;
#1503 = ORIENTED_EDGE('',*,*,#1175,.T.) ;
#1504 = ORIENTED_EDGE('',*,*,#1146,.T.) ;
#1505 = ORIENTED_EDGE('',*,*,#1175,.F.) ;
#1506 = ORIENTED_EDGE('',*,*,#1155,.F.) ;
#1507 = ORIENTED_EDGE('',*,*,#1176,.T.) ;
#1508 = ORIENTED_EDGE('',*,*,#1176,.F.) ;
#1509 = ORIENTED_EDGE('',*,*,#1177,.T.) ;
#1510 = ORIENTED_EDGE('',*,*,#1173,.T.) ;
#1511 = ORIENTED_EDGE('',*,*,#1174,.T.) ;
#1512 = ORIENTED_EDGE('',*,*,#1177,.F.) ;
#1513 = ORIENTED_EDGE('',*,*,#1178,.F.) ;
#1514 = ORIENTED_EDGE('',*,*,#1179,.T.) ;
#1515 = ORIENTED_EDGE('',*,*,#1180,.T.) ;
#1516 = ORIENTED_EDGE('',*,*,#1179,.F.) ;
#1517 = ORIENTED_EDGE('',*,*,#1180,.F.) ;
#1518 = ORIENTED_EDGE('',*,*,#1181,.T.) ;
#1519 = ORIENTED_EDGE('',*,*,#1182,.F.) ;
#1520 = ORIENTED_EDGE('',*,*,#1183,.T.) ;
#1521 = ORIENTED_EDGE('',*,*,#1178,.T.) ;
#1522 = ORIENTED_EDGE('',*,*,#1183,.F.) ;
#1523 = ORIENTED_EDGE('',*,*,#1181,.F.) ;
#1524 = ORIENTED_EDGE('',*,*,#1184,.T.) ;
#1525 = ORIENTED_EDGE('',*,*,#1185,.T.) ;
#1526 = ORIENTED_EDGE('',*,*,#1184,.F.) ;
#1527 = ORIENTED_EDGE('',*,*,#1182,.T.) ;
#1528 = ORIENTED_EDGE('',*,*,#1186,.T.) ;
#1529 = ORIENTED_EDGE('',*,*,#1187,.F.) ;
#1530 = ORIENTED_EDGE('',*,*,#1186,.F.) ;
#1531 = ORIENTED_EDGE('',*,*,#1185,.F.) ;
#1532 = ORIENTED_EDGE('',*,*,#1188,.T.) ;
#1533 = ORIENTED_EDGE('',*,*,#1189,.T.) ;
#1534 = ORIENTED_EDGE('',*,*,#1188,.F.) ;
#1535 = ORIENTED_EDGE('',*,*,#1190,.F.) ;
#1536 = ORIENTED_EDGE('',*,*,#1187,.T.) ;
#1537 = ORIENTED_EDGE('',*,*,#1189,.F.) ;
#1538 = ORIENTED_EDGE('',*,*,#1191,.T.) ;
#1539 = ORIENTED_EDGE('',*,*,#1192,.T.) ;
#1540 = ORIENTED_EDGE('',*,*,#1191,.F.) ;
#1541 = ORIENTED_EDGE('',*,*,#1193,.F.) ;
#1542 = ORIENTED_EDGE('',*,*,#1194,.T.) ;
#1543 = ORIENTED_EDGE('',*,*,#1190,.T.) ;
#1544 = ORIENTED_EDGE('',*,*,#1194,.F.) ;
#1545 = ORIENTED_EDGE('',*,*,#1195,.T.) ;
#1546 = ORIENTED_EDGE('',*,*,#1196,.T.) ;
#1547 = ORIENTED_EDGE('',*,*,#1197,.T.) ;
#1548 = ORIENTED_EDGE('',*,*,#1198,.T.) ;
#1549 = ORIENTED_EDGE('',*,*,#1199,.T.) ;
#1550 = ORIENTED_EDGE('',*,*,#1200,.T.) ;
#1551 = ORIENTED_EDGE('',*,*,#1193,.T.) ;
#1552 = ORIENTED_EDGE('',*,*,#1201,.F.) ;
#1553 = ORIENTED_EDGE('',*,*,#1202,.F.) ;
#1554 = ORIENTED_EDGE('',*,*,#1203,.F.) ;
#1555 = ORIENTED_EDGE('',*,*,#1204,.F.) ;
#1556 = ORIENTED_EDGE('',*,*,#1205,.F.) ;
#1557 = ORIENTED_EDGE('',*,*,#1206,.F.) ;
#1558 = ORIENTED_EDGE('',*,*,#1207,.F.) ;
#1559 = ORIENTED_EDGE('',*,*,#1202,.T.) ;
#1560 = ORIENTED_EDGE('',*,*,#1208,.F.) ;
#1561 = ORIENTED_EDGE('',*,*,#1198,.F.) ;
#1562 = ORIENTED_EDGE('',*,*,#1209,.T.) ;
#1563 = ORIENTED_EDGE('',*,*,#1210,.F.) ;
#1564 = ORIENTED_EDGE('',*,*,#1211,.F.) ;
#1565 = ORIENTED_EDGE('',*,*,#1212,.F.) ;
#1566 = ORIENTED_EDGE('',*,*,#1213,.F.) ;
#1567 = ORIENTED_EDGE('',*,*,#1214,.F.) ;
#1568 = ORIENTED_EDGE('',*,*,#1212,.T.) ;
#1569 = ORIENTED_EDGE('',*,*,#1215,.T.) ;
#1570 = ORIENTED_EDGE('',*,*,#1216,.F.) ;
#1571 = ORIENTED_EDGE('',*,*,#1217,.F.) ;
#1572 = ORIENTED_EDGE('',*,*,#1213,.T.) ;
#1573 = ORIENTED_EDGE('',*,*,#1214,.T.) ;
#1574 = ORIENTED_EDGE('',*,*,#1218,.F.) ;
#1575 = ORIENTED_EDGE('',*,*,#1215,.F.) ;
#1576 = ORIENTED_EDGE('',*,*,#1211,.T.) ;
#1577 = ORIENTED_EDGE('',*,*,#1219,.T.) ;
#1578 = ORIENTED_EDGE('',*,*,#1220,.F.) ;
#1579 = ORIENTED_EDGE('',*,*,#1216,.T.) ;
#1580 = ORIENTED_EDGE('',*,*,#1220,.T.) ;
#1581 = ORIENTED_EDGE('',*,*,#1221,.T.) ;
#1582 = ORIENTED_EDGE('',*,*,#1218,.T.) ;
#1583 = ORIENTED_EDGE('',*,*,#1219,.F.) ;
#1584 = ORIENTED_EDGE('',*,*,#1210,.T.) ;
#1585 = ORIENTED_EDGE('',*,*,#1217,.T.) ;
#1586 = ORIENTED_EDGE('',*,*,#1221,.F.) ;
#1587 = ORIENTED_EDGE('',*,*,#1203,.T.) ;
#1588 = ORIENTED_EDGE('',*,*,#1209,.F.) ;
#1589 = ORIENTED_EDGE('',*,*,#1197,.F.) ;
#1590 = ORIENTED_EDGE('',*,*,#1222,.T.) ;
#1591 = ORIENTED_EDGE('',*,*,#1223,.F.) ;
#1592 = ORIENTED_EDGE('',*,*,#1224,.F.) ;
#1593 = ORIENTED_EDGE('',*,*,#1225,.F.) ;
#1594 = ORIENTED_EDGE('',*,*,#1226,.F.) ;
#1595 = ORIENTED_EDGE('',*,*,#1201,.T.) ;
#1596 = ORIENTED_EDGE('',*,*,#1227,.F.) ;
#1597 = ORIENTED_EDGE('',*,*,#1199,.F.) ;
#1598 = ORIENTED_EDGE('',*,*,#1208,.T.) ;
#1599 = ORIENTED_EDGE('',*,*,#1228,.F.) ;
#1600 = ORIENTED_EDGE('',*,*,#1229,.F.) ;
#1601 = ORIENTED_EDGE('',*,*,#1230,.F.) ;
#1602 = ORIENTED_EDGE('',*,*,#1231,.F.) ;
#1603 = ORIENTED_EDGE('',*,*,#1204,.T.) ;
#1604 = ORIENTED_EDGE('',*,*,#1222,.F.) ;
#1605 = ORIENTED_EDGE('',*,*,#1196,.F.) ;
#1606 = ORIENTED_EDGE('',*,*,#1232,.T.) ;
#1607 = ORIENTED_EDGE('',*,*,#1233,.F.) ;
#1608 = ORIENTED_EDGE('',*,*,#1234,.F.) ;
#1609 = ORIENTED_EDGE('',*,*,#1235,.F.) ;
#1610 = ORIENTED_EDGE('',*,*,#1236,.F.) ;
#1611 = ORIENTED_EDGE('',*,*,#1206,.T.) ;
#1612 = ORIENTED_EDGE('',*,*,#1237,.F.) ;
#1613 = ORIENTED_EDGE('',*,*,#1200,.F.) ;
#1614 = ORIENTED_EDGE('',*,*,#1227,.T.) ;
#1615 = ORIENTED_EDGE('',*,*,#1238,.F.) ;
#1616 = ORIENTED_EDGE('',*,*,#1239,.F.) ;
#1617 = ORIENTED_EDGE('',*,*,#1240,.F.) ;
#1618 = ORIENTED_EDGE('',*,*,#1241,.F.) ;
#1619 = ORIENTED_EDGE('',*,*,#1205,.T.) ;
#1620 = ORIENTED_EDGE('',*,*,#1232,.F.) ;
#1621 = ORIENTED_EDGE('',*,*,#1195,.F.) ;
#1622 = ORIENTED_EDGE('',*,*,#1237,.T.) ;
#1623 = ORIENTED_EDGE('',*,*,#1242,.F.) ;
#1624 = ORIENTED_EDGE('',*,*,#1243,.F.) ;
#1625 = ORIENTED_EDGE('',*,*,#1244,.F.) ;
#1626 = ORIENTED_EDGE('',*,*,#1245,.F.) ;
#1627 = ORIENTED_EDGE('',*,*,#1246,.F.) ;
#1628 = ORIENTED_EDGE('',*,*,#1243,.T.) ;
#1629 = ORIENTED_EDGE('',*,*,#1247,.T.) ;
#1630 = ORIENTED_EDGE('',*,*,#1248,.F.) ;
#1631 = ORIENTED_EDGE('',*,*,#1249,.F.) ;
#1632 = ORIENTED_EDGE('',*,*,#1244,.T.) ;
#1633 = ORIENTED_EDGE('',*,*,#1246,.T.) ;
#1634 = ORIENTED_EDGE('',*,*,#1250,.F.) ;
#1635 = ORIENTED_EDGE('',*,*,#1247,.F.) ;
#1636 = ORIENTED_EDGE('',*,*,#1242,.T.) ;
#1637 = ORIENTED_EDGE('',*,*,#1251,.T.) ;
#1638 = ORIENTED_EDGE('',*,*,#1252,.F.) ;
#1639 = ORIENTED_EDGE('',*,*,#1248,.T.) ;
#1640 = ORIENTED_EDGE('',*,*,#1252,.T.) ;
#1641 = ORIENTED_EDGE('',*,*,#1253,.T.) ;
#1642 = ORIENTED_EDGE('',*,*,#1250,.T.) ;
#1643 = ORIENTED_EDGE('',*,*,#1251,.F.) ;
#1644 = ORIENTED_EDGE('',*,*,#1245,.T.) ;
#1645 = ORIENTED_EDGE('',*,*,#1249,.T.) ;
#1646 = ORIENTED_EDGE('',*,*,#1253,.F.) ;
#1647 = ORIENTED_EDGE('',*,*,#1254,.F.) ;
#1648 = ORIENTED_EDGE('',*,*,#1229,.T.) ;
#1649 = ORIENTED_EDGE('',*,*,#1255,.T.) ;
#1650 = ORIENTED_EDGE('',*,*,#1256,.F.) ;
#1651 = ORIENTED_EDGE('',*,*,#1257,.F.) ;
#1652 = ORIENTED_EDGE('',*,*,#1230,.T.) ;
#1653 = ORIENTED_EDGE('',*,*,#1254,.T.) ;
#1654 = ORIENTED_EDGE('',*,*,#1258,.F.) ;
#1655 = ORIENTED_EDGE('',*,*,#1255,.F.) ;
#1656 = ORIENTED_EDGE('',*,*,#1228,.T.) ;
#1657 = ORIENTED_EDGE('',*,*,#1259,.T.) ;
#1658 = ORIENTED_EDGE('',*,*,#1260,.F.) ;
#1659 = ORIENTED_EDGE('',*,*,#1256,.T.) ;
#1660 = ORIENTED_EDGE('',*,*,#1260,.T.) ;
#1661 = ORIENTED_EDGE('',*,*,#1261,.T.) ;
#1662 = ORIENTED_EDGE('',*,*,#1258,.T.) ;
#1663 = ORIENTED_EDGE('',*,*,#1259,.F.) ;
#1664 = ORIENTED_EDGE('',*,*,#1231,.T.) ;
#1665 = ORIENTED_EDGE('',*,*,#1257,.T.) ;
#1666 = ORIENTED_EDGE('',*,*,#1261,.F.) ;
#1667 = ORIENTED_EDGE('',*,*,#1262,.F.) ;
#1668 = ORIENTED_EDGE('',*,*,#1234,.T.) ;
#1669 = ORIENTED_EDGE('',*,*,#1263,.T.) ;
#1670 = ORIENTED_EDGE('',*,*,#1264,.F.) ;
#1671 = ORIENTED_EDGE('',*,*,#1265,.F.) ;
#1672 = ORIENTED_EDGE('',*,*,#1235,.T.) ;
#1673 = ORIENTED_EDGE('',*,*,#1262,.T.) ;
#1674 = ORIENTED_EDGE('',*,*,#1266,.F.) ;
#1675 = ORIENTED_EDGE('',*,*,#1263,.F.) ;
#1676 = ORIENTED_EDGE('',*,*,#1233,.T.) ;
#1677 = ORIENTED_EDGE('',*,*,#1267,.T.) ;
#1678 = ORIENTED_EDGE('',*,*,#1268,.F.) ;
#1679 = ORIENTED_EDGE('',*,*,#1264,.T.) ;
#1680 = ORIENTED_EDGE('',*,*,#1268,.T.) ;
#1681 = ORIENTED_EDGE('',*,*,#1269,.T.) ;
#1682 = ORIENTED_EDGE('',*,*,#1266,.T.) ;
#1683 = ORIENTED_EDGE('',*,*,#1267,.F.) ;
#1684 = ORIENTED_EDGE('',*,*,#1236,.T.) ;
#1685 = ORIENTED_EDGE('',*,*,#1265,.T.) ;
#1686 = ORIENTED_EDGE('',*,*,#1269,.F.) ;
#1687 = ORIENTED_EDGE('',*,*,#1270,.F.) ;
#1688 = ORIENTED_EDGE('',*,*,#1224,.T.) ;
#1689 = ORIENTED_EDGE('',*,*,#1271,.T.) ;
#1690 = ORIENTED_EDGE('',*,*,#1272,.F.) ;
#1691 = ORIENTED_EDGE('',*,*,#1273,.F.) ;
#1692 = ORIENTED_EDGE('',*,*,#1225,.T.) ;
#1693 = ORIENTED_EDGE('',*,*,#1270,.T.) ;
#1694 = ORIENTED_EDGE('',*,*,#1274,.F.) ;
#1695 = ORIENTED_EDGE('',*,*,#1271,.F.) ;
#1696 = ORIENTED_EDGE('',*,*,#1223,.T.) ;
#1697 = ORIENTED_EDGE('',*,*,#1275,.T.) ;
#1698 = ORIENTED_EDGE('',*,*,#1276,.F.) ;
#1699 = ORIENTED_EDGE('',*,*,#1272,.T.) ;
#1700 = ORIENTED_EDGE('',*,*,#1276,.T.) ;
#1701 = ORIENTED_EDGE('',*,*,#1277,.T.) ;
#1702 = ORIENTED_EDGE('',*,*,#1274,.T.) ;
#1703 = ORIENTED_EDGE('',*,*,#1275,.F.) ;
#1704 = ORIENTED_EDGE('',*,*,#1226,.T.) ;
#1705 = ORIENTED_EDGE('',*,*,#1273,.T.) ;
#1706 = ORIENTED_EDGE('',*,*,#1277,.F.) ;
#1707 = ORIENTED_EDGE('',*,*,#1278,.F.) ;
#1708 = ORIENTED_EDGE('',*,*,#1239,.T.) ;
#1709 = ORIENTED_EDGE('',*,*,#1279,.T.) ;
#1710 = ORIENTED_EDGE('',*,*,#1280,.F.) ;
#1711 = ORIENTED_EDGE('',*,*,#1281,.F.) ;
#1712 = ORIENTED_EDGE('',*,*,#1240,.T.) ;
#1713 = ORIENTED_EDGE('',*,*,#1278,.T.) ;
#1714 = ORIENTED_EDGE('',*,*,#1282,.F.) ;
#1715 = ORIENTED_EDGE('',*,*,#1279,.F.) ;
#1716 = ORIENTED_EDGE('',*,*,#1238,.T.) ;
#1717 = ORIENTED_EDGE('',*,*,#1283,.T.) ;
#1718 = ORIENTED_EDGE('',*,*,#1284,.F.) ;
#1719 = ORIENTED_EDGE('',*,*,#1280,.T.) ;
#1720 = ORIENTED_EDGE('',*,*,#1284,.T.) ;
#1721 = ORIENTED_EDGE('',*,*,#1285,.T.) ;
#1722 = ORIENTED_EDGE('',*,*,#1282,.T.) ;
#1723 = ORIENTED_EDGE('',*,*,#1283,.F.) ;
#1724 = ORIENTED_EDGE('',*,*,#1241,.T.) ;
#1725 = ORIENTED_EDGE('',*,*,#1281,.T.) ;
#1726 = ORIENTED_EDGE('',*,*,#1285,.F.) ;
#1727 = ORIENTED_EDGE('',*,*,#1286,.T.) ;
#1728 = ORIENTED_EDGE('',*,*,#1192,.F.) ;
#1729 = ORIENTED_EDGE('',*,*,#1286,.F.) ;
#1730 = ORIENTED_EDGE('',*,*,#1287,.T.) ;
#1731 = ORIENTED_EDGE('',*,*,#1288,.T.) ;
#1732 = ORIENTED_EDGE('',*,*,#1289,.T.) ;
#1733 = ORIENTED_EDGE('',*,*,#1287,.F.) ;
#1734 = ORIENTED_EDGE('',*,*,#1290,.T.) ;
#1735 = ORIENTED_EDGE('',*,*,#1291,.T.) ;
#1736 = ORIENTED_EDGE('',*,*,#1207,.T.) ;
#1737 = ORIENTED_EDGE('',*,*,#1291,.F.) ;
#1738 = ORIENTED_EDGE('',*,*,#1292,.T.) ;
#1739 = ORIENTED_EDGE('',*,*,#1289,.F.) ;
#1740 = ORIENTED_EDGE('',*,*,#1293,.T.) ;
#1741 = ORIENTED_EDGE('',*,*,#1294,.F.) ;
#1742 = ORIENTED_EDGE('',*,*,#1295,.F.) ;
#1743 = ORIENTED_EDGE('',*,*,#1293,.F.) ;
#1744 = ORIENTED_EDGE('',*,*,#1288,.F.) ;
#1745 = ORIENTED_EDGE('',*,*,#1294,.T.) ;
#1746 = ORIENTED_EDGE('',*,*,#1295,.T.) ;
#1747 = ORIENTED_EDGE('',*,*,#1296,.T.) ;
#1748 = ORIENTED_EDGE('',*,*,#1292,.F.) ;
#1749 = ORIENTED_EDGE('',*,*,#1290,.F.) ;
#1750 = ORIENTED_EDGE('',*,*,#1296,.F.) ;
#1751 = ORIENTED_EDGE('',*,*,#1297,.F.) ;
#1752 = ORIENTED_EDGE('',*,*,#1298,.T.) ;
#1753 = ORIENTED_EDGE('',*,*,#1299,.T.) ;
#1754 = ORIENTED_EDGE('',*,*,#1298,.F.) ;
#1755 = ORIENTED_EDGE('',*,*,#1300,.F.) ;
#1756 = ORIENTED_EDGE('',*,*,#1301,.T.) ;
#1757 = ORIENTED_EDGE('',*,*,#1302,.T.) ;
#1758 = ORIENTED_EDGE('',*,*,#1301,.F.) ;
#1759 = ORIENTED_EDGE('',*,*,#1300,.T.) ;
#1760 = ORIENTED_EDGE('',*,*,#1303,.T.) ;
#1761 = ORIENTED_EDGE('',*,*,#1304,.F.) ;
#1762 = ORIENTED_EDGE('',*,*,#1303,.F.) ;
#1763 = ORIENTED_EDGE('',*,*,#1305,.F.) ;
#1764 = ORIENTED_EDGE('',*,*,#1306,.T.) ;
#1765 = ORIENTED_EDGE('',*,*,#1304,.T.) ;
#1766 = ORIENTED_EDGE('',*,*,#1306,.F.) ;
#1767 = ORIENTED_EDGE('',*,*,#1305,.T.) ;
#1768 = ORIENTED_EDGE('',*,*,#1307,.T.) ;
#1769 = ORIENTED_EDGE('',*,*,#1308,.F.) ;
#1770 = ORIENTED_EDGE('',*,*,#1307,.F.) ;
#1771 = ORIENTED_EDGE('',*,*,#1309,.F.) ;
#1772 = ORIENTED_EDGE('',*,*,#1310,.T.) ;
#1773 = ORIENTED_EDGE('',*,*,#1311,.T.) ;
#1774 = ORIENTED_EDGE('',*,*,#1310,.F.) ;
#1775 = ORIENTED_EDGE('',*,*,#1312,.F.) ;
#1776 = ORIENTED_EDGE('',*,*,#1313,.T.) ;
#1777 = ORIENTED_EDGE('',*,*,#1309,.T.) ;
#1778 = ORIENTED_EDGE('',*,*,#1313,.F.) ;
#1779 = ORIENTED_EDGE('',*,*,#1312,.T.) ;
#1780 = ORIENTED_EDGE('',*,*,#1314,.T.) ;
#1781 = ORIENTED_EDGE('',*,*,#1315,.F.) ;
#1782 = ORIENTED_EDGE('',*,*,#1314,.F.) ;
#1783 = ORIENTED_EDGE('',*,*,#1316,.F.) ;
#1784 = ORIENTED_EDGE('',*,*,#1317,.T.) ;
#1785 = ORIENTED_EDGE('',*,*,#1315,.T.) ;
#1786 = ORIENTED_EDGE('',*,*,#1317,.F.) ;
#1787 = ORIENTED_EDGE('',*,*,#1318,.F.) ;
#1788 = ORIENTED_EDGE('',*,*,#1319,.T.) ;
#1789 = ORIENTED_EDGE('',*,*,#1320,.T.) ;
#1790 = ORIENTED_EDGE('',*,*,#1319,.F.) ;
#1791 = ORIENTED_EDGE('',*,*,#1321,.F.) ;
#1792 = ORIENTED_EDGE('',*,*,#1322,.T.) ;
#1793 = ORIENTED_EDGE('',*,*,#1318,.T.) ;
#1794 = ORIENTED_EDGE('',*,*,#1322,.F.) ;
#1795 = ORIENTED_EDGE('',*,*,#1321,.T.) ;
#1796 = ORIENTED_EDGE('',*,*,#1323,.T.) ;
#1797 = ORIENTED_EDGE('',*,*,#1324,.F.) ;
#1798 = ORIENTED_EDGE('',*,*,#1323,.F.) ;
#1799 = ORIENTED_EDGE('',*,*,#1325,.F.) ;
#1800 = ORIENTED_EDGE('',*,*,#1326,.T.) ;
#1801 = ORIENTED_EDGE('',*,*,#1324,.T.) ;
#1802 = ORIENTED_EDGE('',*,*,#1326,.F.) ;
#1803 = ORIENTED_EDGE('',*,*,#1325,.T.) ;
#1804 = ORIENTED_EDGE('',*,*,#1327,.T.) ;
#1805 = ORIENTED_EDGE('',*,*,#1328,.F.) ;
#1806 = ORIENTED_EDGE('',*,*,#1327,.F.) ;
#1807 = ORIENTED_EDGE('',*,*,#1297,.T.) ;
#1808 = ORIENTED_EDGE('',*,*,#1302,.F.) ;
#1809 = ORIENTED_EDGE('',*,*,#1308,.T.) ;
#1810 = ORIENTED_EDGE('',*,*,#1311,.F.) ;
#1811 = ORIENTED_EDGE('',*,*,#1320,.F.) ;
#1812 = ORIENTED_EDGE('',*,*,#1316,.T.) ;
#1813 = ORIENTED_EDGE('',*,*,#1299,.F.) ;
#1814 = ORIENTED_EDGE('',*,*,#1328,.T.) ;
#1815 = ORIENTED_EDGE('',*,*,#1329,.F.) ;
#1816 = ORIENTED_EDGE('',*,*,#1330,.T.) ;
#1817 = ORIENTED_EDGE('',*,*,#1331,.T.) ;
#1818 = ORIENTED_EDGE('',*,*,#1330,.F.) ;
#1819 = ORIENTED_EDGE('',*,*,#1332,.F.) ;
#1820 = ORIENTED_EDGE('',*,*,#1333,.T.) ;
#1821 = ORIENTED_EDGE('',*,*,#1334,.T.) ;
#1822 = ORIENTED_EDGE('',*,*,#1333,.F.) ;
#1823 = ORIENTED_EDGE('',*,*,#1334,.F.) ;
#1824 = ORIENTED_EDGE('',*,*,#1335,.T.) ;
#1825 = ORIENTED_EDGE('',*,*,#1336,.T.) ;
#1826 = ORIENTED_EDGE('',*,*,#1337,.T.) ;
#1827 = ORIENTED_EDGE('',*,*,#1335,.F.) ;
#1828 = ORIENTED_EDGE('',*,*,#1337,.F.) ;
#1829 = ORIENTED_EDGE('',*,*,#1336,.F.) ;
#1830 = ORIENTED_EDGE('',*,*,#1338,.T.) ;
#1831 = ORIENTED_EDGE('',*,*,#1339,.T.) ;
#1832 = ORIENTED_EDGE('',*,*,#1338,.F.) ;
#1833 = ORIENTED_EDGE('',*,*,#1340,.T.) ;
#1834 = ORIENTED_EDGE('',*,*,#1339,.F.) ;
#1835 = ORIENTED_EDGE('',*,*,#1340,.F.) ;
#1836 = ORIENTED_EDGE('',*,*,#1341,.T.) ;
#1837 = ORIENTED_EDGE('',*,*,#1342,.T.) ;
#1838 = ORIENTED_EDGE('',*,*,#1341,.F.) ;
#1839 = ORIENTED_EDGE('',*,*,#1343,.F.) ;
#1840 = ORIENTED_EDGE('',*,*,#1344,.T.) ;
#1841 = ORIENTED_EDGE('',*,*,#1345,.T.) ;
#1842 = ORIENTED_EDGE('',*,*,#1344,.F.) ;
#1843 = ORIENTED_EDGE('',*,*,#1346,.T.) ;
#1844 = ORIENTED_EDGE('',*,*,#1345,.F.) ;
#1845 = ORIENTED_EDGE('',*,*,#1346,.F.) ;
#1846 = ORIENTED_EDGE('',*,*,#1347,.T.) ;
#1847 = ORIENTED_EDGE('',*,*,#1348,.T.) ;
#1848 = ORIENTED_EDGE('',*,*,#1347,.F.) ;
#1849 = ORIENTED_EDGE('',*,*,#1348,.F.) ;
#1850 = ORIENTED_EDGE('',*,*,#1349,.T.) ;
#1851 = ORIENTED_EDGE('',*,*,#1349,.F.) ;
#1852 = ORIENTED_EDGE('',*,*,#1350,.T.) ;
#1853 = ORIENTED_EDGE('',*,*,#1351,.T.) ;
#1854 = ORIENTED_EDGE('',*,*,#1350,.F.) ;
#1855 = ORIENTED_EDGE('',*,*,#1351,.F.) ;
#1856 = ORIENTED_EDGE('',*,*,#1329,.T.) ;
#1857 = ORIENTED_EDGE('',*,*,#1332,.T.) ;
#1858 = ORIENTED_EDGE('',*,*,#1352,.T.) ;
#1859 = ORIENTED_EDGE('',*,*,#1353,.T.) ;
#1860 = ORIENTED_EDGE('',*,*,#1343,.T.) ;
#1861 = ORIENTED_EDGE('',*,*,#1354,.T.) ;
#1862 = ORIENTED_EDGE('',*,*,#1342,.F.) ;
#1863 = ORIENTED_EDGE('',*,*,#1354,.F.) ;
#1864 = ORIENTED_EDGE('',*,*,#1355,.F.) ;
#1865 = ORIENTED_EDGE('',*,*,#1356,.F.) ;
#1866 = ORIENTED_EDGE('',*,*,#1357,.F.) ;
#1867 = ORIENTED_EDGE('',*,*,#1358,.F.) ;
#1868 = ORIENTED_EDGE('',*,*,#1331,.F.) ;
#1869 = ORIENTED_EDGE('',*,*,#1352,.F.) ;
#1870 = ORIENTED_EDGE('',*,*,#1359,.T.) ;
#1871 = ORIENTED_EDGE('',*,*,#1356,.T.) ;
#1872 = ORIENTED_EDGE('',*,*,#1355,.T.) ;
#1873 = ORIENTED_EDGE('',*,*,#1359,.F.) ;
#1874 = ORIENTED_EDGE('',*,*,#1353,.F.) ;
#1875 = ORIENTED_EDGE('',*,*,#1360,.T.) ;
#1876 = ORIENTED_EDGE('',*,*,#1358,.T.) ;
#1877 = ORIENTED_EDGE('',*,*,#1357,.T.) ;
#1878 = ORIENTED_EDGE('',*,*,#1360,.F.) ;
#1879 = ORIENTED_EDGE('',*,*,#1361,.F.) ;
#1880 = ORIENTED_EDGE('',*,*,#1362,.T.) ;
#1881 = ORIENTED_EDGE('',*,*,#1363,.T.) ;
#1882 = ORIENTED_EDGE('',*,*,#1364,.F.) ;
#1883 = ORIENTED_EDGE('',*,*,#1365,.T.) ;
#1884 = ORIENTED_EDGE('',*,*,#1366,.T.) ;
#1885 = ORIENTED_EDGE('',*,*,#1367,.T.) ;
#1886 = ORIENTED_EDGE('',*,*,#1364,.T.) ;
#1887 = ORIENTED_EDGE('',*,*,#1367,.F.) ;
#1888 = ORIENTED_EDGE('',*,*,#1368,.T.) ;
#1889 = ORIENTED_EDGE('',*,*,#1369,.T.) ;
#1890 = ORIENTED_EDGE('',*,*,#1366,.F.) ;
#1891 = ORIENTED_EDGE('',*,*,#1370,.F.) ;
#1892 = ORIENTED_EDGE('',*,*,#1371,.T.) ;
#1893 = ORIENTED_EDGE('',*,*,#1370,.T.) ;
#1894 = ORIENTED_EDGE('',*,*,#1365,.F.) ;
#1895 = ORIENTED_EDGE('',*,*,#1369,.F.) ;
#1896 = ORIENTED_EDGE('',*,*,#1372,.T.) ;
#1897 = ORIENTED_EDGE('',*,*,#1373,.T.) ;
#1898 = ORIENTED_EDGE('',*,*,#1361,.T.) ;
#1899 = ORIENTED_EDGE('',*,*,#1373,.F.) ;
#1900 = ORIENTED_EDGE('',*,*,#1374,.T.) ;
#1901 = ORIENTED_EDGE('',*,*,#1375,.T.) ;
#1902 = ORIENTED_EDGE('',*,*,#1376,.T.) ;
#1903 = ORIENTED_EDGE('',*,*,#1374,.F.) ;
#1904 = ORIENTED_EDGE('',*,*,#1372,.F.) ;
#1905 = ORIENTED_EDGE('',*,*,#1376,.F.) ;
#1906 = ORIENTED_EDGE('',*,*,#1377,.T.) ;
#1907 = ORIENTED_EDGE('',*,*,#1363,.F.) ;
#1908 = ORIENTED_EDGE('',*,*,#1378,.T.) ;
#1909 = ORIENTED_EDGE('',*,*,#1379,.T.) ;
#1910 = ORIENTED_EDGE('',*,*,#1380,.T.) ;
#1911 = ORIENTED_EDGE('',*,*,#1378,.F.) ;
#1912 = ORIENTED_EDGE('',*,*,#1381,.F.) ;
#1913 = ORIENTED_EDGE('',*,*,#1382,.F.) ;
#1914 = ORIENTED_EDGE('',*,*,#1383,.T.) ;
#1915 = ORIENTED_EDGE('',*,*,#1377,.F.) ;
#1916 = ORIENTED_EDGE('',*,*,#1375,.F.) ;
#1917 = ORIENTED_EDGE('',*,*,#1383,.F.) ;
#1918 = ORIENTED_EDGE('',*,*,#1384,.T.) ;
#1919 = ORIENTED_EDGE('',*,*,#1382,.T.) ;
#1920 = ORIENTED_EDGE('',*,*,#1385,.F.) ;
#1921 = ORIENTED_EDGE('',*,*,#1379,.F.) ;
#1922 = ORIENTED_EDGE('',*,*,#1385,.T.) ;
#1923 = ORIENTED_EDGE('',*,*,#1381,.T.) ;
#1924 = ORIENTED_EDGE('',*,*,#1384,.F.) ;
#1925 = ORIENTED_EDGE('',*,*,#1380,.F.) ;
#1926 = ORIENTED_EDGE('',*,*,#1362,.F.) ;
#1927 = ORIENTED_EDGE('',*,*,#1386,.T.) ;
#1928 = ORIENTED_EDGE('',*,*,#1387,.T.) ;
#1929 = ORIENTED_EDGE('',*,*,#1386,.F.) ;
#1930 = ORIENTED_EDGE('',*,*,#1388,.F.) ;
#1931 = ORIENTED_EDGE('',*,*,#1389,.T.) ;
#1932 = ORIENTED_EDGE('',*,*,#1368,.F.) ;
#1933 = ORIENTED_EDGE('',*,*,#1371,.F.) ;
#1934 = ORIENTED_EDGE('',*,*,#1389,.F.) ;
#1935 = ORIENTED_EDGE('',*,*,#1388,.T.) ;
#1936 = ORIENTED_EDGE('',*,*,#1390,.T.) ;
#1937 = ORIENTED_EDGE('',*,*,#1387,.F.) ;
#1938 = ORIENTED_EDGE('',*,*,#1390,.F.) ;
#1939 = ORIENTED_EDGE('',*,*,#1391,.F.) ;
#1940 = ORIENTED_EDGE('',*,*,#1392,.T.) ;
#1941 = ORIENTED_EDGE('',*,*,#1393,.T.) ;
#1942 = ORIENTED_EDGE('',*,*,#1392,.F.) ;
#1943 = ORIENTED_EDGE('',*,*,#1394,.F.) ;
#1944 = ORIENTED_EDGE('',*,*,#1395,.T.) ;
#1945 = ORIENTED_EDGE('',*,*,#1391,.T.) ;
#1946 = ORIENTED_EDGE('',*,*,#1395,.F.) ;
#1947 = ORIENTED_EDGE('',*,*,#1396,.F.) ;
#1948 = ORIENTED_EDGE('',*,*,#1397,.T.) ;
#1949 = ORIENTED_EDGE('',*,*,#1394,.T.) ;
#1950 = ORIENTED_EDGE('',*,*,#1397,.F.) ;
#1951 = ORIENTED_EDGE('',*,*,#1396,.T.) ;
#1952 = ORIENTED_EDGE('',*,*,#1398,.T.) ;
#1953 = ORIENTED_EDGE('',*,*,#1399,.F.) ;
#1954 = ORIENTED_EDGE('',*,*,#1398,.F.) ;
#1955 = ORIENTED_EDGE('',*,*,#1400,.F.) ;
#1956 = ORIENTED_EDGE('',*,*,#1401,.T.) ;
#1957 = ORIENTED_EDGE('',*,*,#1399,.T.) ;
#1958 = ORIENTED_EDGE('',*,*,#1401,.F.) ;
#1959 = ORIENTED_EDGE('',*,*,#1402,.T.) ;
#1960 = ORIENTED_EDGE('',*,*,#1393,.F.) ;
#1961 = ORIENTED_EDGE('',*,*,#1402,.F.) ;
#1962 = ORIENTED_EDGE('',*,*,#1403,.T.) ;
#1963 = ORIENTED_EDGE('',*,*,#1404,.T.) ;
#1964 = ORIENTED_EDGE('',*,*,#1405,.T.) ;
#1965 = ORIENTED_EDGE('',*,*,#1403,.F.) ;
#1966 = ORIENTED_EDGE('',*,*,#1405,.F.) ;
#1967 = ORIENTED_EDGE('',*,*,#1406,.T.) ;
#1968 = ORIENTED_EDGE('',*,*,#1407,.F.) ;
#1969 = ORIENTED_EDGE('',*,*,#1408,.F.) ;
#1970 = ORIENTED_EDGE('',*,*,#1406,.F.) ;
#1971 = ORIENTED_EDGE('',*,*,#1404,.F.) ;
#1972 = ORIENTED_EDGE('',*,*,#1407,.T.) ;
#1973 = ORIENTED_EDGE('',*,*,#1408,.T.) ;
#1974 = ORIENTED_EDGE('',*,*,#1409,.T.) ;
#1975 = ORIENTED_EDGE('',*,*,#1410,.F.) ;
#1976 = ORIENTED_EDGE('',*,*,#1411,.F.) ;
#1977 = ORIENTED_EDGE('',*,*,#1409,.F.) ;
#1978 = ORIENTED_EDGE('',*,*,#1410,.T.) ;
#1979 = ORIENTED_EDGE('',*,*,#1411,.T.) ;
#1980 = ORIENTED_EDGE('',*,*,#1412,.T.) ;
#1981 = ORIENTED_EDGE('',*,*,#1413,.F.) ;
#1982 = ORIENTED_EDGE('',*,*,#1414,.F.) ;
#1983 = ORIENTED_EDGE('',*,*,#1412,.F.) ;
#1984 = ORIENTED_EDGE('',*,*,#1413,.T.) ;
#1985 = ORIENTED_EDGE('',*,*,#1414,.T.) ;
#1986 = ORIENTED_EDGE('',*,*,#1415,.T.) ;
#1987 = ORIENTED_EDGE('',*,*,#1416,.F.) ;
#1988 = ORIENTED_EDGE('',*,*,#1417,.F.) ;
#1989 = ORIENTED_EDGE('',*,*,#1415,.F.) ;
#1990 = ORIENTED_EDGE('',*,*,#1418,.F.) ;
#1991 = ORIENTED_EDGE('',*,*,#1419,.F.) ;
#1992 = ORIENTED_EDGE('',*,*,#1420,.T.) ;
#1993 = ORIENTED_EDGE('',*,*,#1421,.T.) ;
#1994 = ORIENTED_EDGE('',*,*,#1420,.F.) ;
#1995 = ORIENTED_EDGE('',*,*,#1422,.T.) ;
#1996 = ORIENTED_EDGE('',*,*,#1423,.T.) ;
#1997 = ORIENTED_EDGE('',*,*,#1416,.T.) ;
#1998 = ORIENTED_EDGE('',*,*,#1417,.T.) ;
#1999 = ORIENTED_EDGE('',*,*,#1423,.F.) ;
#2000 = ORIENTED_EDGE('',*,*,#1424,.F.) ;
#2001 = ORIENTED_EDGE('',*,*,#1425,.T.) ;
#2002 = ORIENTED_EDGE('',*,*,#1418,.T.) ;
#2003 = ORIENTED_EDGE('',*,*,#1419,.T.) ;
#2004 = ORIENTED_EDGE('',*,*,#1425,.F.) ;
#2005 = ORIENTED_EDGE('',*,*,#1424,.T.) ;
#2006 = ORIENTED_EDGE('',*,*,#1426,.T.) ;
#2007 = ORIENTED_EDGE('',*,*,#1422,.F.) ;
#2008 = ORIENTED_EDGE('',*,*,#1426,.F.) ;
#2009 = ORIENTED_EDGE('',*,*,#1427,.F.) ;
#2010 = ORIENTED_EDGE('',*,*,#1428,.T.) ;
#2011 = ORIENTED_EDGE('',*,*,#1400,.T.) ;
#2012 = ORIENTED_EDGE('',*,*,#1428,.F.) ;
#2013 = ORIENTED_EDGE('',*,*,#1421,.F.) ;
#2014 = ORIENTED_EDGE('',*,*,#1429,.T.) ;
#2015 = ORIENTED_EDGE('',*,*,#1429,.F.) ;
#2016 = ORIENTED_EDGE('',*,*,#1430,.T.) ;
#2017 = ORIENTED_EDGE('',*,*,#1427,.T.) ;
#2018 = ORIENTED_EDGE('',*,*,#1430,.F.) ;
#2019 = SPHERICAL_SURFACE('',#2215,6.5000000000005) ;
#2020 = SPHERICAL_SURFACE('',#2225,6.5000000000005) ;
#2021 = SPHERICAL_SURFACE('',#2238,8.20000000000063) ;
#2022 = SPHERICAL_SURFACE('',#2246,8.20000000000063) ;
#2023 = SPHERICAL_SURFACE('',#2360,6.5000000000005) ;
#2024 = SPHERICAL_SURFACE('',#2478,6.5) ;
#2025 = SPHERICAL_SURFACE('',#2487,6.5) ;
#2026 = ADVANCED_FACE('',(#480),#2019,.F.) ;
#2027 = ADVANCED_FACE('',(#481),#461,.F.) ;
#2028 = ADVANCED_FACE('',(#482),#177,.F.) ;
#2029 = ADVANCED_FACE('',(#483),#462,.F.) ;
#2030 = ADVANCED_FACE('',(#484),#2020,.F.) ;
#2031 = ADVANCED_FACE('',(#485),#161,.T.) ;
#2032 = ADVANCED_FACE('',(#486),#162,.T.) ;
#2033 = ADVANCED_FACE('',(#487),#2021,.T.) ;
#2034 = ADVANCED_FACE('',(#488),#163,.F.) ;
#2035 = ADVANCED_FACE('',(#489),#2022,.T.) ;
#2036 = ADVANCED_FACE('',(#490),#178,.T.) ;
#2037 = ADVANCED_FACE('',(#491),#164,.F.) ;
#2038 = ADVANCED_FACE('',(#492),#179,.F.) ;
#2039 = ADVANCED_FACE('',(#493,#85),#117,.T.) ;
#2040 = ADVANCED_FACE('',(#494),#165,.T.) ;
#2041 = ADVANCED_FACE('',(#495),#180,.F.) ;
#2042 = ADVANCED_FACE('',(#496,#86),#118,.F.) ;
#2043 = ADVANCED_FACE('',(#497),#166,.T.) ;
#2044 = ADVANCED_FACE('',(#498),#463,.T.) ;
#2045 = ADVANCED_FACE('',(#499,#87),#119,.F.) ;
#2046 = ADVANCED_FACE('',(#500),#181,.T.) ;
#2047 = ADVANCED_FACE('',(#501),#182,.F.) ;
#2048 = ADVANCED_FACE('',(#502),#464,.T.) ;
#2049 = ADVANCED_FACE('',(#503),#465,.F.) ;
#2050 = ADVANCED_FACE('',(#504,#88),#120,.F.) ;
#2051 = ADVANCED_FACE('',(#505),#183,.F.) ;
#2052 = ADVANCED_FACE('',(#506),#184,.T.) ;
#2053 = ADVANCED_FACE('',(#507,#89),#121,.F.) ;
#2054 = ADVANCED_FACE('',(#508,#90),#122,.T.) ;
#2055 = ADVANCED_FACE('',(#509,#91),#123,.F.) ;
#2056 = ADVANCED_FACE('',(#510),#185,.F.) ;
#2057 = ADVANCED_FACE('',(#511),#124,.F.) ;
#2058 = ADVANCED_FACE('',(#512),#125,.F.) ;
#2059 = ADVANCED_FACE('',(#513),#126,.T.) ;
#2060 = ADVANCED_FACE('',(#514),#186,.F.) ;
#2061 = ADVANCED_FACE('',(#515,#92),#127,.F.) ;
#2062 = ADVANCED_FACE('',(#516,#93),#128,.F.) ;
#2063 = ADVANCED_FACE('',(#517,#94),#129,.F.) ;
#2064 = ADVANCED_FACE('',(#518,#95),#130,.F.) ;
#2065 = ADVANCED_FACE('',(#519,#96),#131,.F.) ;
#2066 = ADVANCED_FACE('',(#520),#187,.F.) ;
#2067 = ADVANCED_FACE('',(#521),#132,.F.) ;
#2068 = ADVANCED_FACE('',(#522),#133,.F.) ;
#2069 = ADVANCED_FACE('',(#523),#134,.T.) ;
#2070 = ADVANCED_FACE('',(#524),#188,.F.) ;
#2071 = ADVANCED_FACE('',(#525),#189,.F.) ;
#2072 = ADVANCED_FACE('',(#526),#135,.F.) ;
#2073 = ADVANCED_FACE('',(#527),#136,.F.) ;
#2074 = ADVANCED_FACE('',(#528),#137,.T.) ;
#2075 = ADVANCED_FACE('',(#529),#190,.F.) ;
#2076 = ADVANCED_FACE('',(#530),#191,.F.) ;
#2077 = ADVANCED_FACE('',(#531),#138,.F.) ;
#2078 = ADVANCED_FACE('',(#532),#139,.F.) ;
#2079 = ADVANCED_FACE('',(#533),#140,.T.) ;
#2080 = ADVANCED_FACE('',(#534),#192,.F.) ;
#2081 = ADVANCED_FACE('',(#535),#193,.F.) ;
#2082 = ADVANCED_FACE('',(#536),#141,.F.) ;
#2083 = ADVANCED_FACE('',(#537),#142,.F.) ;
#2084 = ADVANCED_FACE('',(#538),#143,.T.) ;
#2085 = ADVANCED_FACE('',(#539),#194,.F.) ;
#2086 = ADVANCED_FACE('',(#540),#195,.F.) ;
#2087 = ADVANCED_FACE('',(#541),#144,.F.) ;
#2088 = ADVANCED_FACE('',(#542),#145,.F.) ;
#2089 = ADVANCED_FACE('',(#543),#146,.T.) ;
#2090 = ADVANCED_FACE('',(#544),#196,.F.) ;
#2091 = ADVANCED_FACE('',(#545,#97),#147,.T.) ;
#2092 = ADVANCED_FACE('',(#546),#167,.T.) ;
#2093 = ADVANCED_FACE('',(#547),#197,.T.) ;
#2094 = ADVANCED_FACE('',(#548),#2023,.T.) ;
#2095 = ADVANCED_FACE('',(#549),#168,.F.) ;
#2096 = ADVANCED_FACE('',(#550),#198,.T.) ;
#2097 = ADVANCED_FACE('',(#551),#199,.T.) ;
#2098 = ADVANCED_FACE('',(#552),#466,.T.) ;
#2099 = ADVANCED_FACE('',(#553),#200,.T.) ;
#2100 = ADVANCED_FACE('',(#554),#467,.T.) ;
#2101 = ADVANCED_FACE('',(#555),#468,.F.) ;
#2102 = ADVANCED_FACE('',(#556),#201,.F.) ;
#2103 = ADVANCED_FACE('',(#557),#469,.F.) ;
#2104 = ADVANCED_FACE('',(#558),#202,.F.) ;
#2105 = ADVANCED_FACE('',(#559),#470,.F.) ;
#2106 = ADVANCED_FACE('',(#560),#203,.F.) ;
#2107 = ADVANCED_FACE('',(#561),#471,.F.) ;
#2108 = ADVANCED_FACE('',(#562),#204,.F.) ;
#2109 = ADVANCED_FACE('',(#563),#472,.F.) ;
#2110 = ADVANCED_FACE('',(#564,#98),#148,.T.) ;
#2111 = ADVANCED_FACE('',(#565,#99),#149,.T.) ;
#2112 = ADVANCED_FACE('',(#566,#100),#150,.F.) ;
#2113 = ADVANCED_FACE('',(#567,#101),#151,.F.) ;
#2114 = ADVANCED_FACE('',(#568),#205,.F.) ;
#2115 = ADVANCED_FACE('',(#569),#206,.T.) ;
#2116 = ADVANCED_FACE('',(#570,#102),#152,.F.) ;
#2117 = ADVANCED_FACE('',(#571),#473,.F.) ;
#2118 = ADVANCED_FACE('',(#572),#207,.F.) ;
#2119 = ADVANCED_FACE('',(#573,#103),#153,.T.) ;
#2120 = ADVANCED_FACE('',(#574),#208,.T.) ;
#2121 = ADVANCED_FACE('',(#575),#209,.T.) ;
#2122 = ADVANCED_FACE('',(#576,#104),#154,.T.) ;
#2123 = ADVANCED_FACE('',(#577),#210,.T.) ;
#2124 = ADVANCED_FACE('',(#578,#105),#155,.F.) ;
#2125 = ADVANCED_FACE('',(#579),#211,.T.) ;
#2126 = ADVANCED_FACE('',(#580,#106,#107,#108,#109),#156,.F.) ;
#2127 = ADVANCED_FACE('',(#581,#110,#111,#112),#474,.T.) ;
#2128 = ADVANCED_FACE('',(#582),#212,.F.) ;
#2129 = ADVANCED_FACE('',(#583),#213,.F.) ;
#2130 = ADVANCED_FACE('',(#584,#113),#157,.F.) ;
#2131 = ADVANCED_FACE('',(#585,#114),#158,.T.) ;
#2132 = ADVANCED_FACE('',(#586),#214,.F.) ;
#2133 = ADVANCED_FACE('',(#587),#55,.F.) ;
#2134 = ADVANCED_FACE('',(#588),#56,.F.) ;
#2135 = ADVANCED_FACE('',(#589),#215,.T.) ;
#2136 = ADVANCED_FACE('',(#590),#169,.F.) ;
#2137 = ADVANCED_FACE('',(#591),#216,.T.) ;
#2138 = ADVANCED_FACE('',(#592),#475,.T.) ;
#2139 = ADVANCED_FACE('',(#593),#57,.T.) ;
#2140 = ADVANCED_FACE('',(#594),#58,.T.) ;
#2141 = ADVANCED_FACE('',(#595),#217,.F.) ;
#2142 = ADVANCED_FACE('',(#596),#476,.F.) ;
#2143 = ADVANCED_FACE('',(#597),#170,.T.) ;
#2144 = ADVANCED_FACE('',(#598),#218,.F.) ;
#2145 = ADVANCED_FACE('',(#599),#477,.F.) ;
#2146 = ADVANCED_FACE('',(#600),#219,.F.) ;
#2147 = ADVANCED_FACE('',(#601),#478,.F.) ;
#2148 = ADVANCED_FACE('',(#602),#2024,.F.) ;
#2149 = ADVANCED_FACE('',(#603,#115),#159,.T.) ;
#2150 = ADVANCED_FACE('',(#604),#171,.T.) ;
#2151 = ADVANCED_FACE('',(#605),#2025,.T.) ;
#2152 = ADVANCED_FACE('',(#606),#172,.F.) ;
#2153 = ADVANCED_FACE('',(#607),#220,.T.) ;
#2154 = ADVANCED_FACE('',(#608),#173,.F.) ;
#2155 = ADVANCED_FACE('',(#609),#174,.T.) ;
#2156 = ADVANCED_FACE('',(#610),#479,.T.) ;
#2157 = ADVANCED_FACE('',(#611),#221,.T.) ;
#2158 = ADVANCED_FACE('',(#612),#175,.T.) ;
#2159 = ADVANCED_FACE('',(#613),#222,.F.) ;
#2160 = ADVANCED_FACE('',(#614,#116),#160,.F.) ;
#2161 = ADVANCED_FACE('',(#615),#176,.T.) ;
#2162 = CLOSED_SHELL('',(#2026,#2027,#2028,#2029,#2030,#2031,#2032,#2033,
#2034,#2035,#2036,#2037,#2038,#2039,#2040,#2041,#2042,#2043)) ;
#2163 = CLOSED_SHELL('',(#2044,#2045,#2046,#2047,#2048,#2049,#2050,#2051,
#2052,#2053,#2054,#2055,#2056,#2057,#2058,#2059,#2060,#2061,#2062,#2063,
#2064,#2065,#2066,#2067,#2068,#2069,#2070,#2071,#2072,#2073,#2074,#2075,
#2076,#2077,#2078,#2079,#2080,#2081,#2082,#2083,#2084,#2085,#2086,#2087,
#2088,#2089,#2090,#2091,#2092,#2093,#2094,#2095)) ;
#2164 = CLOSED_SHELL('',(#2096,#2097,#2098,#2099,#2100,#2101,#2102,#2103,
#2104,#2105,#2106,#2107,#2108,#2109,#2110,#2111,#2112,#2113)) ;
#2165 = CLOSED_SHELL('',(#2114,#2115,#2116,#2117,#2118,#2119,#2120,#2121,
#2122,#2123,#2124,#2125,#2126,#2127,#2128,#2129)) ;
#2166 = CLOSED_SHELL('',(#2130,#2131,#2132,#2133,#2134,#2135,#2136,#2137,
#2138,#2139,#2140,#2141,#2142,#2143)) ;
#2167 = CLOSED_SHELL('',(#2144,#2145,#2146,#2147,#2148,#2149,#2150,#2151,
#2152,#2153,#2154,#2155,#2156,#2157,#2158,#2159,#2160,#2161)) ;
#2168 = DERIVED_UNIT_ELEMENT(#2176,1.) ;
#2169 = DERIVED_UNIT_ELEMENT(#4306,-3.) ;
#2170 = DERIVED_UNIT_ELEMENT(#2176,1.) ;
#2171 = DERIVED_UNIT_ELEMENT(#4306,-3.) ;
#2172 = DERIVED_UNIT_ELEMENT(#2176,1.) ;
#2173 = DERIVED_UNIT_ELEMENT(#4306,-3.) ;
#2174 = DERIVED_UNIT_ELEMENT(#2176,1.) ;
#2175 = DERIVED_UNIT_ELEMENT(#4306,-3.) ;
#2176 = (
MASS_UNIT()
NAMED_UNIT(*)
SI_UNIT(.KILO.,.GRAM.)
) ;
#2177 = DERIVED_UNIT((#2168,#2169)) ;
#2178 = DERIVED_UNIT((#2170,#2171)) ;
#2179 = DERIVED_UNIT((#2172,#2173)) ;
#2180 = DERIVED_UNIT((#2174,#2175)) ;
#2181 = MEASURE_REPRESENTATION_ITEM('density measure',
POSITIVE_RATIO_MEASURE(7850.),#2177) ;
#2182 = MEASURE_REPRESENTATION_ITEM('density measure',
POSITIVE_RATIO_MEASURE(7850.),#2178) ;
#2183 = MEASURE_REPRESENTATION_ITEM('density measure',
POSITIVE_RATIO_MEASURE(7850.),#2179) ;
#2184 = MEASURE_REPRESENTATION_ITEM('density measure',
POSITIVE_RATIO_MEASURE(7850.),#2180) ;
#2185 = PROPERTY_DEFINITION_REPRESENTATION(#2205,#2193) ;
#2186 = PROPERTY_DEFINITION_REPRESENTATION(#2206,#2194) ;
#2187 = PROPERTY_DEFINITION_REPRESENTATION(#2207,#2195) ;
#2188 = PROPERTY_DEFINITION_REPRESENTATION(#2208,#2196) ;
#2189 = PROPERTY_DEFINITION_REPRESENTATION(#2209,#2197) ;
#2190 = PROPERTY_DEFINITION_REPRESENTATION(#2210,#2198) ;
#2191 = PROPERTY_DEFINITION_REPRESENTATION(#2211,#2199) ;
#2192 = PROPERTY_DEFINITION_REPRESENTATION(#2212,#2200) ;
#2193 = REPRESENTATION('material name',(#2201),#4300) ;
#2194 = REPRESENTATION('density',(#2181),#4300) ;
#2195 = REPRESENTATION('material name',(#2202),#4301) ;
#2196 = REPRESENTATION('density',(#2182),#4301) ;
#2197 = REPRESENTATION('material name',(#2203),#4302) ;
#2198 = REPRESENTATION('density',(#2183),#4302) ;
#2199 = REPRESENTATION('material name',(#2204),#4303) ;
#2200 = REPRESENTATION('density',(#2184),#4303) ;
#2201 = DESCRIPTIVE_REPRESENTATION_ITEM('Steel','Steel') ;
#2202 = DESCRIPTIVE_REPRESENTATION_ITEM('Steel','Steel') ;
#2203 = DESCRIPTIVE_REPRESENTATION_ITEM('Steel','Steel') ;
#2204 = DESCRIPTIVE_REPRESENTATION_ITEM('Steel','Steel') ;
#2205 = PROPERTY_DEFINITION('material property','material name',#4337) ;
#2206 = PROPERTY_DEFINITION('material property','density of part',#4337) ;
#2207 = PROPERTY_DEFINITION('material property','material name',#4338) ;
#2208 = PROPERTY_DEFINITION('material property','density of part',#4338) ;
#2209 = PROPERTY_DEFINITION('material property','material name',#4339) ;
#2210 = PROPERTY_DEFINITION('material property','density of part',#4339) ;
#2211 = PROPERTY_DEFINITION('material property','material name',#4340) ;
#2212 = PROPERTY_DEFINITION('material property','density of part',#4340) ;
#2213 = AXIS2_PLACEMENT_3D('',#3283,#2530,#2531) ;
#2214 = AXIS2_PLACEMENT_3D('',#3284,#2532,#2533) ;
#2215 = AXIS2_PLACEMENT_3D('',#3285,#2534,#2535) ;
#2216 = AXIS2_PLACEMENT_3D('',#3287,#2536,#2537) ;
#2217 = AXIS2_PLACEMENT_3D('',#3289,#2538,#2539) ;
#2218 = AXIS2_PLACEMENT_3D('',#3290,#2540,#2541) ;
#2219 = AXIS2_PLACEMENT_3D('',#3291,#2542,#2543) ;
#2220 = AXIS2_PLACEMENT_3D('',#3293,#2544,#2545) ;
#2221 = AXIS2_PLACEMENT_3D('',#3295,#2547,#2548) ;
#2222 = AXIS2_PLACEMENT_3D('',#3297,#2549,#2550) ;
#2223 = AXIS2_PLACEMENT_3D('',#3299,#2552,#2553) ;
#2224 = AXIS2_PLACEMENT_3D('',#3302,#2555,#2556) ;
#2225 = AXIS2_PLACEMENT_3D('',#3303,#2557,#2558) ;
#2226 = AXIS2_PLACEMENT_3D('',#3305,#2559,#2560) ;
#2227 = AXIS2_PLACEMENT_3D('',#3306,#2561,#2562) ;
#2228 = AXIS2_PLACEMENT_3D('',#3307,#2563,#2564) ;
#2229 = AXIS2_PLACEMENT_3D('',#3309,#2565,#2566) ;
#2230 = AXIS2_PLACEMENT_3D('',#3311,#2567,#2568) ;
#2231 = AXIS2_PLACEMENT_3D('',#3313,#2569,#2570) ;
#2232 = AXIS2_PLACEMENT_3D('',#3314,#2571,#2572) ;
#2233 = AXIS2_PLACEMENT_3D('',#3315,#2573,#2574) ;
#2234 = AXIS2_PLACEMENT_3D('',#3318,#2575,#2576) ;
#2235 = AXIS2_PLACEMENT_3D('',#3319,#2577,#2578) ;
#2236 = AXIS2_PLACEMENT_3D('',#3321,#2579,#2580) ;
#2237 = AXIS2_PLACEMENT_3D('',#3322,#2581,#2582) ;
#2238 = AXIS2_PLACEMENT_3D('',#3323,#2583,#2584) ;
#2239 = AXIS2_PLACEMENT_3D('',#3325,#2585,#2586) ;
#2240 = AXIS2_PLACEMENT_3D('',#3327,#2587,#2588) ;
#2241 = AXIS2_PLACEMENT_3D('',#3328,#2589,#2590) ;
#2242 = AXIS2_PLACEMENT_3D('',#3329,#2591,#2592) ;
#2243 = AXIS2_PLACEMENT_3D('',#3331,#2593,#2594) ;
#2244 = AXIS2_PLACEMENT_3D('',#3333,#2595,#2596) ;
#2245 = AXIS2_PLACEMENT_3D('',#3334,#2597,#2598) ;
#2246 = AXIS2_PLACEMENT_3D('',#3335,#2599,#2600) ;
#2247 = AXIS2_PLACEMENT_3D('',#3338,#2601,#2602) ;
#2248 = AXIS2_PLACEMENT_3D('',#3339,#2603,#2604) ;
#2249 = AXIS2_PLACEMENT_3D('',#3340,#2605,#2606) ;
#2250 = AXIS2_PLACEMENT_3D('',#3341,#2607,#2608) ;
#2251 = AXIS2_PLACEMENT_3D('',#3345,#2610,#2611) ;
#2252 = AXIS2_PLACEMENT_3D('',#3346,#2612,#2613) ;
#2253 = AXIS2_PLACEMENT_3D('',#3347,#2614,#2615) ;
#2254 = AXIS2_PLACEMENT_3D('',#3348,#2616,#2617) ;
#2255 = AXIS2_PLACEMENT_3D('',#3349,#2618,#2619) ;
#2256 = AXIS2_PLACEMENT_3D('',#3352,#2621,#2622) ;
#2257 = AXIS2_PLACEMENT_3D('',#3353,#2623,#2624) ;
#2258 = AXIS2_PLACEMENT_3D('',#3355,#2625,#2626) ;
#2259 = AXIS2_PLACEMENT_3D('',#3356,#2627,#2628) ;
#2260 = AXIS2_PLACEMENT_3D('',#3357,#2629,#2630) ;
#2261 = AXIS2_PLACEMENT_3D('',#3358,#2631,#2632) ;
#2262 = AXIS2_PLACEMENT_3D('',#3361,#2633,#2634) ;
#2263 = AXIS2_PLACEMENT_3D('',#3362,#2635,#2636) ;
#2264 = AXIS2_PLACEMENT_3D('',#3364,#2638,#2639) ;
#2265 = AXIS2_PLACEMENT_3D('',#3366,#2640,#2641) ;
#2266 = AXIS2_PLACEMENT_3D('',#3367,#2642,#2643) ;
#2267 = AXIS2_PLACEMENT_3D('',#3368,#2644,#2645) ;
#2268 = AXIS2_PLACEMENT_3D('',#3369,#2646,#2647) ;
#2269 = AXIS2_PLACEMENT_3D('',#3370,#2648,#2649) ;
#2270 = AXIS2_PLACEMENT_3D('',#3372,#2650,#2651) ;
#2271 = AXIS2_PLACEMENT_3D('',#3375,#2653,#2654) ;
#2272 = AXIS2_PLACEMENT_3D('',#3376,#2655,#2656) ;
#2273 = AXIS2_PLACEMENT_3D('',#3378,#2657,#2658) ;
#2274 = AXIS2_PLACEMENT_3D('',#3379,#2659,#2660) ;
#2275 = AXIS2_PLACEMENT_3D('',#3381,#2661,#2662) ;
#2276 = AXIS2_PLACEMENT_3D('',#3383,#2664,#2665) ;
#2277 = AXIS2_PLACEMENT_3D('',#3386,#2667,#2668) ;
#2278 = AXIS2_PLACEMENT_3D('',#3387,#2669,#2670) ;
#2279 = AXIS2_PLACEMENT_3D('',#3390,#2672,#2673) ;
#2280 = AXIS2_PLACEMENT_3D('',#3391,#2674,#2675) ;
#2281 = AXIS2_PLACEMENT_3D('',#3394,#2677,#2678) ;
#2282 = AXIS2_PLACEMENT_3D('',#3395,#2679,#2680) ;
#2283 = AXIS2_PLACEMENT_3D('',#3397,#2681,#2682) ;
#2284 = AXIS2_PLACEMENT_3D('',#3398,#2683,#2684) ;
#2285 = AXIS2_PLACEMENT_3D('',#3401,#2686,#2687) ;
#2286 = AXIS2_PLACEMENT_3D('',#3402,#2688,#2689) ;
#2287 = AXIS2_PLACEMENT_3D('',#3404,#2690,#2691) ;
#2288 = AXIS2_PLACEMENT_3D('',#3406,#2693,#2694) ;
#2289 = AXIS2_PLACEMENT_3D('',#3419,#2701,#2702) ;
#2290 = AXIS2_PLACEMENT_3D('',#3433,#2709,#2710) ;
#2291 = AXIS2_PLACEMENT_3D('',#3434,#2711,#2712) ;
#2292 = AXIS2_PLACEMENT_3D('',#3439,#2715,#2716) ;
#2293 = AXIS2_PLACEMENT_3D('',#3443,#2718,#2719) ;
#2294 = AXIS2_PLACEMENT_3D('',#3445,#2721,#2722) ;
#2295 = AXIS2_PLACEMENT_3D('',#3450,#2725,#2726) ;
#2296 = AXIS2_PLACEMENT_3D('',#3451,#2727,#2728) ;
#2297 = AXIS2_PLACEMENT_3D('',#3455,#2731,#2732) ;
#2298 = AXIS2_PLACEMENT_3D('',#3459,#2735,#2736) ;
#2299 = AXIS2_PLACEMENT_3D('',#3460,#2737,#2738) ;
#2300 = AXIS2_PLACEMENT_3D('',#3461,#2739,#2740) ;
#2301 = AXIS2_PLACEMENT_3D('',#3462,#2741,#2742) ;
#2302 = AXIS2_PLACEMENT_3D('',#3468,#2745,#2746) ;
#2303 = AXIS2_PLACEMENT_3D('',#3471,#2748,#2749) ;
#2304 = AXIS2_PLACEMENT_3D('',#3472,#2750,#2751) ;
#2305 = AXIS2_PLACEMENT_3D('',#3478,#2754,#2755) ;
#2306 = AXIS2_PLACEMENT_3D('',#3481,#2757,#2758) ;
#2307 = AXIS2_PLACEMENT_3D('',#3482,#2759,#2760) ;
#2308 = AXIS2_PLACEMENT_3D('',#3488,#2763,#2764) ;
#2309 = AXIS2_PLACEMENT_3D('',#3491,#2766,#2767) ;
#2310 = AXIS2_PLACEMENT_3D('',#3492,#2768,#2769) ;
#2311 = AXIS2_PLACEMENT_3D('',#3498,#2772,#2773) ;
#2312 = AXIS2_PLACEMENT_3D('',#3501,#2775,#2776) ;
#2313 = AXIS2_PLACEMENT_3D('',#3502,#2777,#2778) ;
#2314 = AXIS2_PLACEMENT_3D('',#3507,#2780,#2781) ;
#2315 = AXIS2_PLACEMENT_3D('',#3510,#2783,#2784) ;
#2316 = AXIS2_PLACEMENT_3D('',#3511,#2785,#2786) ;
#2317 = AXIS2_PLACEMENT_3D('',#3516,#2789,#2790) ;
#2318 = AXIS2_PLACEMENT_3D('',#3517,#2791,#2792) ;
#2319 = AXIS2_PLACEMENT_3D('',#3521,#2795,#2796) ;
#2320 = AXIS2_PLACEMENT_3D('',#3525,#2799,#2800) ;
#2321 = AXIS2_PLACEMENT_3D('',#3526,#2801,#2802) ;
#2322 = AXIS2_PLACEMENT_3D('',#3527,#2803,#2804) ;
#2323 = AXIS2_PLACEMENT_3D('',#3528,#2805,#2806) ;
#2324 = AXIS2_PLACEMENT_3D('',#3533,#2809,#2810) ;
#2325 = AXIS2_PLACEMENT_3D('',#3534,#2811,#2812) ;
#2326 = AXIS2_PLACEMENT_3D('',#3538,#2815,#2816) ;
#2327 = AXIS2_PLACEMENT_3D('',#3542,#2819,#2820) ;
#2328 = AXIS2_PLACEMENT_3D('',#3543,#2821,#2822) ;
#2329 = AXIS2_PLACEMENT_3D('',#3544,#2823,#2824) ;
#2330 = AXIS2_PLACEMENT_3D('',#3545,#2825,#2826) ;
#2331 = AXIS2_PLACEMENT_3D('',#3550,#2829,#2830) ;
#2332 = AXIS2_PLACEMENT_3D('',#3551,#2831,#2832) ;
#2333 = AXIS2_PLACEMENT_3D('',#3555,#2835,#2836) ;
#2334 = AXIS2_PLACEMENT_3D('',#3559,#2839,#2840) ;
#2335 = AXIS2_PLACEMENT_3D('',#3560,#2841,#2842) ;
#2336 = AXIS2_PLACEMENT_3D('',#3561,#2843,#2844) ;
#2337 = AXIS2_PLACEMENT_3D('',#3562,#2845,#2846) ;
#2338 = AXIS2_PLACEMENT_3D('',#3567,#2849,#2850) ;
#2339 = AXIS2_PLACEMENT_3D('',#3568,#2851,#2852) ;
#2340 = AXIS2_PLACEMENT_3D('',#3572,#2855,#2856) ;
#2341 = AXIS2_PLACEMENT_3D('',#3576,#2859,#2860) ;
#2342 = AXIS2_PLACEMENT_3D('',#3577,#2861,#2862) ;
#2343 = AXIS2_PLACEMENT_3D('',#3578,#2863,#2864) ;
#2344 = AXIS2_PLACEMENT_3D('',#3579,#2865,#2866) ;
#2345 = AXIS2_PLACEMENT_3D('',#3584,#2869,#2870) ;
#2346 = AXIS2_PLACEMENT_3D('',#3585,#2871,#2872) ;
#2347 = AXIS2_PLACEMENT_3D('',#3589,#2875,#2876) ;
#2348 = AXIS2_PLACEMENT_3D('',#3593,#2879,#2880) ;
#2349 = AXIS2_PLACEMENT_3D('',#3594,#2881,#2882) ;
#2350 = AXIS2_PLACEMENT_3D('',#3595,#2883,#2884) ;
#2351 = AXIS2_PLACEMENT_3D('',#3596,#2885,#2886) ;
#2352 = AXIS2_PLACEMENT_3D('',#3598,#2887,#2888) ;
#2353 = AXIS2_PLACEMENT_3D('',#3599,#2889,#2890) ;
#2354 = AXIS2_PLACEMENT_3D('',#3601,#2891,#2892) ;
#2355 = AXIS2_PLACEMENT_3D('',#3603,#2893,#2894) ;
#2356 = AXIS2_PLACEMENT_3D('',#3604,#2895,#2896) ;
#2357 = AXIS2_PLACEMENT_3D('',#3605,#2897,#2898) ;
#2358 = AXIS2_PLACEMENT_3D('',#3608,#2899,#2900) ;
#2359 = AXIS2_PLACEMENT_3D('',#3610,#2902,#2903) ;
#2360 = AXIS2_PLACEMENT_3D('',#3611,#2904,#2905) ;
#2361 = AXIS2_PLACEMENT_3D('',#3613,#2906,#2907) ;
#2362 = AXIS2_PLACEMENT_3D('',#3615,#2908,#2909) ;
#2363 = AXIS2_PLACEMENT_3D('',#3616,#2910,#2911) ;
#2364 = AXIS2_PLACEMENT_3D('',#3617,#2912,#2913) ;
#2365 = AXIS2_PLACEMENT_3D('',#3618,#2914,#2915) ;
#2366 = AXIS2_PLACEMENT_3D('',#3619,#2916,#2917) ;
#2367 = AXIS2_PLACEMENT_3D('',#3620,#2918,#2919) ;
#2368 = AXIS2_PLACEMENT_3D('',#3622,#2920,#2921) ;
#2369 = AXIS2_PLACEMENT_3D('',#3625,#2923,#2924) ;
#2370 = AXIS2_PLACEMENT_3D('',#3626,#2925,#2926) ;
#2371 = AXIS2_PLACEMENT_3D('',#3628,#2927,#2928) ;
#2372 = AXIS2_PLACEMENT_3D('',#3631,#2930,#2931) ;
#2373 = AXIS2_PLACEMENT_3D('',#3632,#2932,#2933) ;
#2374 = AXIS2_PLACEMENT_3D('',#3635,#2935,#2936) ;
#2375 = AXIS2_PLACEMENT_3D('',#3636,#2937,#2938) ;
#2376 = AXIS2_PLACEMENT_3D('',#3638,#2939,#2940) ;
#2377 = AXIS2_PLACEMENT_3D('',#3640,#2942,#2943) ;
#2378 = AXIS2_PLACEMENT_3D('',#3643,#2945,#2946) ;
#2379 = AXIS2_PLACEMENT_3D('',#3644,#2947,#2948) ;
#2380 = AXIS2_PLACEMENT_3D('',#3646,#2949,#2950) ;
#2381 = AXIS2_PLACEMENT_3D('',#3649,#2952,#2953) ;
#2382 = AXIS2_PLACEMENT_3D('',#3650,#2954,#2955) ;
#2383 = AXIS2_PLACEMENT_3D('',#3652,#2956,#2957) ;
#2384 = AXIS2_PLACEMENT_3D('',#3654,#2959,#2960) ;
#2385 = AXIS2_PLACEMENT_3D('',#3657,#2962,#2963) ;
#2386 = AXIS2_PLACEMENT_3D('',#3658,#2964,#2965) ;
#2387 = AXIS2_PLACEMENT_3D('',#3660,#2966,#2967) ;
#2388 = AXIS2_PLACEMENT_3D('',#3662,#2969,#2970) ;
#2389 = AXIS2_PLACEMENT_3D('',#3664,#2971,#2972) ;
#2390 = AXIS2_PLACEMENT_3D('',#3667,#2974,#2975) ;
#2391 = AXIS2_PLACEMENT_3D('',#3668,#2976,#2977) ;
#2392 = AXIS2_PLACEMENT_3D('',#3670,#2978,#2979) ;
#2393 = AXIS2_PLACEMENT_3D('',#3672,#2981,#2982) ;
#2394 = AXIS2_PLACEMENT_3D('',#3675,#2984,#2985) ;
#2395 = AXIS2_PLACEMENT_3D('',#3676,#2986,#2987) ;
#2396 = AXIS2_PLACEMENT_3D('',#3678,#2988,#2989) ;
#2397 = AXIS2_PLACEMENT_3D('',#3680,#2991,#2992) ;
#2398 = AXIS2_PLACEMENT_3D('',#3683,#2994,#2995) ;
#2399 = AXIS2_PLACEMENT_3D('',#3684,#2996,#2997) ;
#2400 = AXIS2_PLACEMENT_3D('',#3685,#2998,#2999) ;
#2401 = AXIS2_PLACEMENT_3D('',#3686,#3000,#3001) ;
#2402 = AXIS2_PLACEMENT_3D('',#3687,#3002,#3003) ;
#2403 = AXIS2_PLACEMENT_3D('',#3688,#3004,#3005) ;
#2404 = AXIS2_PLACEMENT_3D('',#3690,#3006,#3007) ;
#2405 = AXIS2_PLACEMENT_3D('',#3731,#3009,#3010) ;
#2406 = AXIS2_PLACEMENT_3D('',#3733,#3011,#3012) ;
#2407 = AXIS2_PLACEMENT_3D('',#3736,#3014,#3015) ;
#2408 = AXIS2_PLACEMENT_3D('',#3737,#3016,#3017) ;
#2409 = AXIS2_PLACEMENT_3D('',#3739,#3018,#3019) ;
#2410 = AXIS2_PLACEMENT_3D('',#3740,#3020,#3021) ;
#2411 = AXIS2_PLACEMENT_3D('',#3742,#3022,#3023) ;
#2412 = AXIS2_PLACEMENT_3D('',#3744,#3025,#3026) ;
#2413 = AXIS2_PLACEMENT_3D('',#3747,#3028,#3029) ;
#2414 = AXIS2_PLACEMENT_3D('',#3748,#3030,#3031) ;
#2415 = AXIS2_PLACEMENT_3D('',#3750,#3032,#3033) ;
#2416 = AXIS2_PLACEMENT_3D('',#3751,#3034,#3035) ;
#2417 = AXIS2_PLACEMENT_3D('',#3754,#3037,#3038) ;
#2418 = AXIS2_PLACEMENT_3D('',#3755,#3039,#3040) ;
#2419 = AXIS2_PLACEMENT_3D('',#3757,#3041,#3042) ;
#2420 = AXIS2_PLACEMENT_3D('',#3760,#3044,#3045) ;
#2421 = AXIS2_PLACEMENT_3D('',#3761,#3046,#3047) ;
#2422 = AXIS2_PLACEMENT_3D('',#3763,#3048,#3049) ;
#2423 = AXIS2_PLACEMENT_3D('',#3764,#3050,#3051) ;
#2424 = AXIS2_PLACEMENT_3D('',#3767,#3053,#3054) ;
#2425 = AXIS2_PLACEMENT_3D('',#3768,#3055,#3056) ;
#2426 = AXIS2_PLACEMENT_3D('',#3770,#3057,#3058) ;
#2427 = AXIS2_PLACEMENT_3D('',#3771,#3059,#3060) ;
#2428 = AXIS2_PLACEMENT_3D('',#3774,#3062,#3063) ;
#2429 = AXIS2_PLACEMENT_3D('',#3775,#3064,#3065) ;
#2430 = AXIS2_PLACEMENT_3D('',#3777,#3066,#3067) ;
#2431 = AXIS2_PLACEMENT_3D('',#3779,#3068,#3069) ;
#2432 = AXIS2_PLACEMENT_3D('',#3780,#3070,#3071) ;
#2433 = AXIS2_PLACEMENT_3D('',#3876,#3073,#3074) ;
#2434 = AXIS2_PLACEMENT_3D('',#3878,#3076,#3077) ;
#2435 = AXIS2_PLACEMENT_3D('',#3880,#3079,#3080) ;
#2436 = AXIS2_PLACEMENT_3D('',#3882,#3081,#3082) ;
#2437 = AXIS2_PLACEMENT_3D('',#3884,#3083,#3084) ;
#2438 = AXIS2_PLACEMENT_3D('',#3885,#3085,#3086) ;
#2439 = AXIS2_PLACEMENT_3D('',#3887,#3087,#3088) ;
#2440 = AXIS2_PLACEMENT_3D('',#3889,#3089,#3090) ;
#2441 = AXIS2_PLACEMENT_3D('',#3890,#3091,#3092) ;
#2442 = AXIS2_PLACEMENT_3D('',#3893,#3093,#3094) ;
#2443 = AXIS2_PLACEMENT_3D('',#3894,#3095,#3096) ;
#2444 = AXIS2_PLACEMENT_3D('',#4025,#3098,#3099) ;
#2445 = AXIS2_PLACEMENT_3D('',#4026,#3100,#3101) ;
#2446 = AXIS2_PLACEMENT_3D('',#4072,#3102,#3103) ;
#2447 = AXIS2_PLACEMENT_3D('',#4073,#3104,#3105) ;
#2448 = AXIS2_PLACEMENT_3D('',#4076,#3106,#3107) ;
#2449 = AXIS2_PLACEMENT_3D('',#4078,#3109,#3110) ;
#2450 = AXIS2_PLACEMENT_3D('',#4079,#3111,#3112) ;
#2451 = AXIS2_PLACEMENT_3D('',#4082,#3113,#3114) ;
#2452 = AXIS2_PLACEMENT_3D('',#4083,#3115,#3116) ;
#2453 = AXIS2_PLACEMENT_3D('',#4084,#3117,#3118) ;
#2454 = AXIS2_PLACEMENT_3D('',#4085,#3119,#3120) ;
#2455 = AXIS2_PLACEMENT_3D('',#4089,#3122,#3123) ;
#2456 = AXIS2_PLACEMENT_3D('',#4090,#3124,#3125) ;
#2457 = AXIS2_PLACEMENT_3D('',#4091,#3126,#3127) ;
#2458 = AXIS2_PLACEMENT_3D('',#4094,#3128,#3129) ;
#2459 = AXIS2_PLACEMENT_3D('',#4095,#3130,#3131) ;
#2460 = AXIS2_PLACEMENT_3D('',#4142,#3133,#3134) ;
#2461 = AXIS2_PLACEMENT_3D('',#4143,#3135,#3136) ;
#2462 = AXIS2_PLACEMENT_3D('',#4189,#3137,#3138) ;
#2463 = AXIS2_PLACEMENT_3D('',#4192,#3140,#3141) ;
#2464 = AXIS2_PLACEMENT_3D('',#4193,#3142,#3143) ;
#2465 = AXIS2_PLACEMENT_3D('',#4195,#3144,#3145) ;
#2466 = AXIS2_PLACEMENT_3D('',#4197,#3147,#3148) ;
#2467 = AXIS2_PLACEMENT_3D('',#4198,#3149,#3150) ;
#2468 = AXIS2_PLACEMENT_3D('',#4199,#3151,#3152) ;
#2469 = AXIS2_PLACEMENT_3D('',#4200,#3153,#3154) ;
#2470 = AXIS2_PLACEMENT_3D('',#4202,#3155,#3156) ;
#2471 = AXIS2_PLACEMENT_3D('',#4205,#3158,#3159) ;
#2472 = AXIS2_PLACEMENT_3D('',#4206,#3160,#3161) ;
#2473 = AXIS2_PLACEMENT_3D('',#4208,#3162,#3163) ;
#2474 = AXIS2_PLACEMENT_3D('',#4210,#3165,#3166) ;
#2475 = AXIS2_PLACEMENT_3D('',#4212,#3167,#3168) ;
#2476 = AXIS2_PLACEMENT_3D('',#4214,#3170,#3171) ;
#2477 = AXIS2_PLACEMENT_3D('',#4217,#3173,#3174) ;
#2478 = AXIS2_PLACEMENT_3D('',#4218,#3175,#3176) ;
#2479 = AXIS2_PLACEMENT_3D('',#4220,#3177,#3178) ;
#2480 = AXIS2_PLACEMENT_3D('',#4221,#3179,#3180) ;
#2481 = AXIS2_PLACEMENT_3D('',#4222,#3181,#3182) ;
#2482 = AXIS2_PLACEMENT_3D('',#4224,#3183,#3184) ;
#2483 = AXIS2_PLACEMENT_3D('',#4225,#3185,#3186) ;
#2484 = AXIS2_PLACEMENT_3D('',#4227,#3187,#3188) ;
#2485 = AXIS2_PLACEMENT_3D('',#4229,#3189,#3190) ;
#2486 = AXIS2_PLACEMENT_3D('',#4230,#3191,#3192) ;
#2487 = AXIS2_PLACEMENT_3D('',#4231,#3193,#3194) ;
#2488 = AXIS2_PLACEMENT_3D('',#4233,#3195,#3196) ;
#2489 = AXIS2_PLACEMENT_3D('',#4235,#3197,#3198) ;
#2490 = AXIS2_PLACEMENT_3D('',#4236,#3199,#3200) ;
#2491 = AXIS2_PLACEMENT_3D('',#4237,#3201,#3202) ;
#2492 = AXIS2_PLACEMENT_3D('',#4239,#3203,#3204) ;
#2493 = AXIS2_PLACEMENT_3D('',#4241,#3205,#3206) ;
#2494 = AXIS2_PLACEMENT_3D('',#4242,#3207,#3208) ;
#2495 = AXIS2_PLACEMENT_3D('',#4243,#3209,#3210) ;
#2496 = AXIS2_PLACEMENT_3D('',#4247,#3212,#3213) ;
#2497 = AXIS2_PLACEMENT_3D('',#4248,#3214,#3215) ;
#2498 = AXIS2_PLACEMENT_3D('',#4249,#3216,#3217) ;
#2499 = AXIS2_PLACEMENT_3D('',#4251,#3218,#3219) ;
#2500 = AXIS2_PLACEMENT_3D('',#4253,#3220,#3221) ;
#2501 = AXIS2_PLACEMENT_3D('',#4254,#3222,#3223) ;
#2502 = AXIS2_PLACEMENT_3D('',#4255,#3224,#3225) ;
#2503 = AXIS2_PLACEMENT_3D('',#4258,#3226,#3227) ;
#2504 = AXIS2_PLACEMENT_3D('',#4259,#3228,#3229) ;
#2505 = AXIS2_PLACEMENT_3D('',#4261,#3230,#3231) ;
#2506 = AXIS2_PLACEMENT_3D('',#4262,#3232,#3233) ;
#2507 = AXIS2_PLACEMENT_3D('',#4263,#3234,#3235) ;
#2508 = AXIS2_PLACEMENT_3D('',#4265,#3236,#3237) ;
#2509 = AXIS2_PLACEMENT_3D('',#4267,#3239,#3240) ;
#2510 = AXIS2_PLACEMENT_3D('',#4269,#3241,#3242) ;
#2511 = AXIS2_PLACEMENT_3D('',#4271,#3244,#3245) ;
#2512 = AXIS2_PLACEMENT_3D('',#4272,#3246,#3247) ;
#2513 = AXIS2_PLACEMENT_3D('',#4273,#3248,#3249) ;
#2514 = AXIS2_PLACEMENT_3D('',#4275,#3250,#3251) ;
#2515 = AXIS2_PLACEMENT_3D('',#4277,#3253,#3254) ;
#2516 = AXIS2_PLACEMENT_3D('',#4279,#3255,#3256) ;
#2517 = AXIS2_PLACEMENT_3D('',#4280,#3257,#3258) ;
#2518 = AXIS2_PLACEMENT_3D('',#4281,#3259,#3260) ;
#2519 = AXIS2_PLACEMENT_3D('',#4282,#3261,#3262) ;
#2520 = AXIS2_PLACEMENT_3D('',#4283,#3263,#3264) ;
#2521 = AXIS2_PLACEMENT_3D('',#4284,#3265,#3266) ;
#2522 = AXIS2_PLACEMENT_3D('',#4285,#3267,#3268) ;
#2523 = AXIS2_PLACEMENT_3D('',#4286,#3269,#3270) ;
#2524 = AXIS2_PLACEMENT_3D('',#4287,#3271,#3272) ;
#2525 = AXIS2_PLACEMENT_3D('',#4288,#3273,#3274) ;
#2526 = AXIS2_PLACEMENT_3D('',#4289,#3275,#3276) ;
#2527 = AXIS2_PLACEMENT_3D('',#4290,#3277,#3278) ;
#2528 = AXIS2_PLACEMENT_3D('',#4291,#3279,#3280) ;
#2529 = AXIS2_PLACEMENT_3D('',#4292,#3281,#3282) ;
#2530 = DIRECTION('axis',(0.,0.,1.)) ;
#2531 = DIRECTION('refdir',(1.,0.,0.)) ;
#2532 = DIRECTION('axis',(0.,0.,1.)) ;
#2533 = DIRECTION('refdir',(1.,0.,0.)) ;
#2534 = DIRECTION('center_axis',(0.855521240266964,-0.510121382366095,0.0886542875724551)) ;
#2535 = DIRECTION('ref_axis',(-0.465119843688757,-0.832406937999121,-0.301267689236458)) ;
#2536 = DIRECTION('center_axis',(0.855521240266964,-0.510121382366096,0.0886542875724545)) ;
#2537 = DIRECTION('ref_axis',(-0.517240562193751,-0.834304337432909,0.190783839363105)) ;
#2538 = DIRECTION('center_axis',(0.227479534154222,0.216506038769898,-0.949409393632244)) ;
#2539 = DIRECTION('ref_axis',(0.465119843688755,0.832406937999122,0.301267689236458)) ;
#2540 = DIRECTION('center_axis',(0.855521240266964,-0.510121382366096,0.0886542875724545)) ;
#2541 = DIRECTION('ref_axis',(-0.517240562193751,-0.834304337432909,0.190783839363105)) ;
#2542 = DIRECTION('center_axis',(0.855521240266964,-0.510121382366096,0.0886542875724545)) ;
#2543 = DIRECTION('ref_axis',(-0.465119843688758,-0.83240693799912,-0.301267689236458)) ;
#2544 = DIRECTION('center_axis',(0.855521240266964,-0.510121382366096,0.0886542875724545)) ;
#2545 = DIRECTION('ref_axis',(-0.517240562193751,-0.834304337432909,0.190783839363105)) ;
#2546 = DIRECTION('',(0.933834265978767,0.22789030186616,0.275716473935178)) ;
#2547 = DIRECTION('center_axis',(0.855521240266964,-0.510121382366096,0.0886542875724545)) ;
#2548 = DIRECTION('ref_axis',(-0.465119843688758,-0.83240693799912,-0.301267689236458)) ;
#2549 = DIRECTION('center_axis',(0.855521240266964,-0.510121382366096,0.0886542875724545)) ;
#2550 = DIRECTION('ref_axis',(-0.517240562193751,-0.834304337432909,0.190783839363105)) ;
#2551 = DIRECTION('',(0.855521240266964,-0.510121382366096,0.0886542875724545)) ;
#2552 = DIRECTION('center_axis',(-0.855521240266964,0.510121382366096,-0.0886542875724545)) ;
#2553 = DIRECTION('ref_axis',(-0.465119843688758,-0.83240693799912,-0.301267689236458)) ;
#2554 = DIRECTION('',(-0.276055474905567,0.949310879265128,0.150340378087632)) ;
#2555 = DIRECTION('center_axis',(-0.855521240266964,0.510121382366096,-0.0886542875724545)) ;
#2556 = DIRECTION('ref_axis',(0.517240562193751,0.834304337432909,-0.190783839363105)) ;
#2557 = DIRECTION('center_axis',(0.855521240266964,-0.510121382366095,0.0886542875724551)) ;
#2558 = DIRECTION('ref_axis',(-0.465119843688757,-0.832406937999121,-0.301267689236458)) ;
#2559 = DIRECTION('center_axis',(0.855521240266964,-0.510121382366096,0.0886542875724545)) ;
#2560 = DIRECTION('ref_axis',(-0.517240562193751,-0.834304337432909,0.190783839363105)) ;
#2561 = DIRECTION('center_axis',(0.227479534154222,0.216506038769898,-0.949409393632244)) ;
#2562 = DIRECTION('ref_axis',(0.465119843688755,0.832406937999122,0.301267689236458)) ;
#2563 = DIRECTION('center_axis',(0.855521240266964,-0.510121382366096,0.0886542875724545)) ;
#2564 = DIRECTION('ref_axis',(0.517704809501169,0.845453579256405,-0.131110547027658)) ;
#2565 = DIRECTION('center_axis',(0.855521240266964,-0.510121382366096,0.0886542875724545)) ;
#2566 = DIRECTION('ref_axis',(-0.517240562193751,-0.834304337432909,0.190783839363105)) ;
#2567 = DIRECTION('center_axis',(0.00807079125203423,-0.158064608864342,-0.987395787793896)) ;
#2568 = DIRECTION('ref_axis',(-0.517704809501169,-0.845453579256405,0.131110547027658)) ;
#2569 = DIRECTION('center_axis',(0.855521240266964,-0.510121382366096,0.0886542875724545)) ;
#2570 = DIRECTION('ref_axis',(-0.517240562193751,-0.834304337432909,0.190783839363105)) ;
#2571 = DIRECTION('center_axis',(0.855521240266964,-0.510121382366096,0.0886542875724545)) ;
#2572 = DIRECTION('ref_axis',(-0.517240562193751,-0.834304337432909,0.190783839363105)) ;
#2573 = DIRECTION('center_axis',(0.855521240266964,-0.510121382366096,0.0886542875724545)) ;
#2574 = DIRECTION('ref_axis',(0.486257491979136,0.850411106325231,0.20088454826805)) ;
#2575 = DIRECTION('center_axis',(0.855521240266964,-0.510121382366096,0.0886542875724545)) ;
#2576 = DIRECTION('ref_axis',(-0.517240562193751,-0.834304337432909,0.190783839363105)) ;
#2577 = DIRECTION('center_axis',(0.855521240266964,-0.510121382366096,0.0886542875724545)) ;
#2578 = DIRECTION('ref_axis',(-0.517240562193751,-0.834304337432909,0.190783839363105)) ;
#2579 = DIRECTION('center_axis',(0.177868094233453,0.128752186356572,-0.975595108414429)) ;
#2580 = DIRECTION('ref_axis',(-0.486257491979132,-0.850411106325233,-0.20088454826805)) ;
#2581 = DIRECTION('center_axis',(0.855521240266964,-0.510121382366096,0.0886542875724545)) ;
#2582 = DIRECTION('ref_axis',(-0.517240562193751,-0.834304337432909,0.190783839363105)) ;
#2583 = DIRECTION('center_axis',(0.855521240266964,-0.510121382366096,0.0886542875724545)) ;
#2584 = DIRECTION('ref_axis',(-0.465119843688757,-0.83240693799912,-0.301267689236459)) ;
#2585 = DIRECTION('center_axis',(-0.227479534154222,-0.2165060387699,0.949409393632244)) ;
#2586 = DIRECTION('ref_axis',(0.465119843688754,0.832406937999121,0.301267689236459)) ;
#2587 = DIRECTION('center_axis',(0.855521240266964,-0.510121382366096,0.0886542875724545)) ;
#2588 = DIRECTION('ref_axis',(-0.517240562193751,-0.834304337432909,0.190783839363105)) ;
#2589 = DIRECTION('center_axis',(0.855521240266964,-0.510121382366096,0.0886542875724545)) ;
#2590 = DIRECTION('ref_axis',(-0.517240562193751,-0.834304337432909,0.190783839363105)) ;
#2591 = DIRECTION('center_axis',(0.855521240266964,-0.510121382366096,0.0886542875724545)) ;
#2592 = DIRECTION('ref_axis',(0.509998973339442,0.800690415698108,-0.314318159516605)) ;
#2593 = DIRECTION('center_axis',(0.0893557756655694,0.314119457312167,0.945169038793122)) ;
#2594 = DIRECTION('ref_axis',(-0.509998973339435,-0.800690415698112,0.314318159516606)) ;
#2595 = DIRECTION('center_axis',(0.855521240266964,-0.510121382366096,0.0886542875724545)) ;
#2596 = DIRECTION('ref_axis',(-0.517240562193751,-0.834304337432909,0.190783839363105)) ;
#2597 = DIRECTION('center_axis',(0.855521240266964,-0.510121382366096,0.0886542875724545)) ;
#2598 = DIRECTION('ref_axis',(-0.517240562193751,-0.834304337432909,0.190783839363105)) ;
#2599 = DIRECTION('center_axis',(0.855521240266964,-0.510121382366096,0.0886542875724545)) ;
#2600 = DIRECTION('ref_axis',(-0.465119843688757,-0.83240693799912,-0.301267689236459)) ;
#2601 = DIRECTION('center_axis',(0.855521240266964,-0.510121382366096,0.0886542875724545)) ;
#2602 = DIRECTION('ref_axis',(-0.517240562193751,-0.834304337432909,0.190783839363105)) ;
#2603 = DIRECTION('center_axis',(-0.227479534154222,-0.2165060387699,0.949409393632244)) ;
#2604 = DIRECTION('ref_axis',(0.465119843688754,0.832406937999121,0.301267689236459)) ;
#2605 = DIRECTION('center_axis',(0.855521240266964,-0.510121382366096,0.0886542875724545)) ;
#2606 = DIRECTION('ref_axis',(-0.517240562193751,-0.834304337432909,0.190783839363105)) ;
#2607 = DIRECTION('center_axis',(0.855521240266964,-0.510121382366096,0.0886542875724545)) ;
#2608 = DIRECTION('ref_axis',(-0.465119843688758,-0.83240693799912,-0.301267689236458)) ;
#2609 = DIRECTION('',(-0.855521240266964,0.510121382366096,-0.0886542875724545)) ;
#2610 = DIRECTION('center_axis',(0.855521240266964,-0.510121382366096,0.0886542875724545)) ;
#2611 = DIRECTION('ref_axis',(-0.517240562193751,-0.834304337432909,0.190783839363105)) ;
#2612 = DIRECTION('center_axis',(0.855521240266964,-0.510121382366096,0.0886542875724545)) ;
#2613 = DIRECTION('ref_axis',(-0.517240562193751,-0.834304337432909,0.190783839363105)) ;
#2614 = DIRECTION('center_axis',(0.855521240266964,-0.510121382366096,0.0886542875724545)) ;
#2615 = DIRECTION('ref_axis',(0.509998973339442,0.800690415698108,-0.314318159516605)) ;
#2616 = DIRECTION('center_axis',(0.0893557756655694,0.314119457312167,0.945169038793122)) ;
#2617 = DIRECTION('ref_axis',(-0.509998973339435,-0.800690415698112,0.314318159516606)) ;
#2618 = DIRECTION('center_axis',(0.855521240266964,-0.510121382366096,0.0886542875724545)) ;
#2619 = DIRECTION('ref_axis',(-0.465119843688758,-0.83240693799912,-0.301267689236458)) ;
#2620 = DIRECTION('',(0.855521240266964,-0.510121382366096,0.0886542875724545)) ;
#2621 = DIRECTION('center_axis',(0.855521240266964,-0.510121382366096,0.0886542875724545)) ;
#2622 = DIRECTION('ref_axis',(-0.517240562193751,-0.834304337432909,0.190783839363105)) ;
#2623 = DIRECTION('center_axis',(0.855521240266964,-0.510121382366096,0.0886542875724545)) ;
#2624 = DIRECTION('ref_axis',(0.0233582592152953,0.20907522041968,0.977620552122803)) ;
#2625 = DIRECTION('center_axis',(0.855521240266964,-0.510121382366096,0.0886542875724545)) ;
#2626 = DIRECTION('ref_axis',(-0.517240562193751,-0.834304337432909,0.190783839363105)) ;
#2627 = DIRECTION('center_axis',(0.855521240266964,-0.510121382366096,0.0886542875724545)) ;
#2628 = DIRECTION('ref_axis',(-0.465119843688758,-0.83240693799912,-0.301267689236458)) ;
#2629 = DIRECTION('center_axis',(-0.227479534154222,-0.216506038769899,0.949409393632244)) ;
#2630 = DIRECTION('ref_axis',(0.465119843688755,0.832406937999121,0.301267689236459)) ;
#2631 = DIRECTION('center_axis',(0.855521240266964,-0.510121382366096,0.0886542875724545)) ;
#2632 = DIRECTION('ref_axis',(-0.465119843688758,-0.83240693799912,-0.301267689236458)) ;
#2633 = DIRECTION('center_axis',(0.855521240266964,-0.510121382366096,0.0886542875724545)) ;
#2634 = DIRECTION('ref_axis',(-0.517240562193751,-0.834304337432909,0.190783839363105)) ;
#2635 = DIRECTION('center_axis',(0.855521240266964,-0.510121382366096,0.0886542875724545)) ;
#2636 = DIRECTION('ref_axis',(-0.517240562193751,-0.834304337432909,0.190783839363105)) ;
#2637 = DIRECTION('',(0.855521240266964,-0.510121382366096,0.0886542875724545)) ;
#2638 = DIRECTION('center_axis',(0.855521240266964,-0.510121382366096,0.0886542875724545)) ;
#2639 = DIRECTION('ref_axis',(0.0233582592152953,0.20907522041968,0.977620552122803)) ;
#2640 = DIRECTION('center_axis',(0.855521240266964,-0.510121382366096,0.0886542875724545)) ;
#2641 = DIRECTION('ref_axis',(-0.517240562193751,-0.834304337432909,0.190783839363105)) ;
#2642 = DIRECTION('center_axis',(0.855521240266963,-0.510121382366096,0.0886542875724557)) ;
#2643 = DIRECTION('ref_axis',(0.484971795675454,0.849467667676745,0.207863029351437)) ;
#2644 = DIRECTION('center_axis',(0.181344326769277,0.134836407638048,-0.974132115436024)) ;
#2645 = DIRECTION('ref_axis',(-0.484971795675455,-0.849467667676745,-0.207863029351437)) ;
#2646 = DIRECTION('axis',(0.,0.,1.)) ;
#2647 = DIRECTION('refdir',(1.,0.,0.)) ;
#2648 = DIRECTION('center_axis',(-0.855521240266964,0.510121382366096,-0.0886542875724541)) ;
#2649 = DIRECTION('ref_axis',(0.442722751678459,0.631934937682125,-0.636124830267568)) ;
#2650 = DIRECTION('center_axis',(-0.855521240266964,0.510121382366096,-0.0886542875724541)) ;
#2651 = DIRECTION('ref_axis',(0.517240562193751,0.834304337432909,-0.190783839363105)) ;
#2652 = DIRECTION('',(0.811169769918609,0.292211018391187,-0.506573119204895)) ;
#2653 = DIRECTION('center_axis',(-0.855521240266964,0.510121382366096,-0.0886542875724541)) ;
#2654 = DIRECTION('ref_axis',(0.517240562193751,0.834304337432909,-0.190783839363105)) ;
#2655 = DIRECTION('center_axis',(-0.855521240266964,0.510121382366096,-0.0886542875724541)) ;
#2656 = DIRECTION('ref_axis',(0.0233582592152952,0.209075220419679,0.977620552122803)) ;
#2657 = DIRECTION('center_axis',(-0.855521240266964,0.510121382366096,-0.0886542875724541)) ;
#2658 = DIRECTION('ref_axis',(0.517240562193751,0.834304337432909,-0.190783839363105)) ;
#2659 = DIRECTION('center_axis',(-0.855521240266964,0.510121382366096,-0.0886542875724541)) ;
#2660 = DIRECTION('ref_axis',(0.442722751678459,0.631934937682125,-0.636124830267568)) ;
#2661 = DIRECTION('center_axis',(-0.855521240266964,0.510121382366096,-0.0886542875724541)) ;
#2662 = DIRECTION('ref_axis',(0.517240562193751,0.834304337432909,-0.190783839363105)) ;
#2663 = DIRECTION('',(0.855521240266964,-0.510121382366096,0.0886542875724541)) ;
#2664 = DIRECTION('center_axis',(-0.855521240266964,0.510121382366096,-0.0886542875724541)) ;
#2665 = DIRECTION('ref_axis',(0.442722751678459,0.631934937682125,-0.636124830267568)) ;
#2666 = DIRECTION('',(-0.855521240266964,0.510121382366096,-0.0886542875724541)) ;
#2667 = DIRECTION('center_axis',(-0.855521240266964,0.510121382366096,-0.0886542875724541)) ;
#2668 = DIRECTION('ref_axis',(0.517240562193751,0.834304337432909,-0.190783839363105)) ;
#2669 = DIRECTION('center_axis',(0.855521240266964,-0.510121382366096,0.0886542875724541)) ;
#2670 = DIRECTION('ref_axis',(0.442722751678459,0.631934937682125,-0.636124830267568)) ;
#2671 = DIRECTION('',(-0.0443514703433129,0.802332400754277,-0.595227406776826)) ;
#2672 = DIRECTION('center_axis',(0.855521240266964,-0.510121382366096,0.0886542875724541)) ;
#2673 = DIRECTION('ref_axis',(-0.517240562193751,-0.834304337432909,0.190783839363105)) ;
#2674 = DIRECTION('center_axis',(-0.855521240266964,0.510121382366096,-0.0886542875724541)) ;
#2675 = DIRECTION('ref_axis',(0.442722751678459,0.631934937682125,-0.636124830267568)) ;
#2676 = DIRECTION('',(-0.917997130339433,-0.0861351910040448,0.387120133239365)) ;
#2677 = DIRECTION('center_axis',(-0.855521240266964,0.510121382366096,-0.0886542875724541)) ;
#2678 = DIRECTION('ref_axis',(0.517240562193751,0.834304337432909,-0.190783839363105)) ;
#2679 = DIRECTION('center_axis',(-0.855521240266964,0.510121382366096,-0.0886542875724541)) ;
#2680 = DIRECTION('ref_axis',(0.0233582592152952,0.209075220419679,0.977620552122803)) ;
#2681 = DIRECTION('center_axis',(-0.855521240266964,0.510121382366096,-0.0886542875724541)) ;
#2682 = DIRECTION('ref_axis',(0.517240562193751,0.834304337432909,-0.190783839363105)) ;
#2683 = DIRECTION('center_axis',(-0.855521240266964,0.510121382366096,-0.0886542875724541)) ;
#2684 = DIRECTION('ref_axis',(0.442722751678459,0.631934937682125,-0.636124830267568)) ;
#2685 = DIRECTION('',(-0.855521240266964,0.510121382366096,-0.0886542875724541)) ;
#2686 = DIRECTION('center_axis',(-0.855521240266964,0.510121382366096,-0.0886542875724541)) ;
#2687 = DIRECTION('ref_axis',(0.517240562193751,0.834304337432909,-0.190783839363105)) ;
#2688 = DIRECTION('center_axis',(-0.855521240266964,0.510121382366096,-0.0886542875724541)) ;
#2689 = DIRECTION('ref_axis',(0.442722751678459,0.631934937682125,-0.636124830267568)) ;
#2690 = DIRECTION('center_axis',(-0.855521240266964,0.510121382366096,-0.0886542875724541)) ;
#2691 = DIRECTION('ref_axis',(0.517240562193751,0.834304337432909,-0.190783839363105)) ;
#2692 = DIRECTION('',(0.855521240266964,-0.510121382366096,0.0886542875724541)) ;
#2693 = DIRECTION('center_axis',(-0.855521240266964,0.510121382366096,-0.0886542875724541)) ;
#2694 = DIRECTION('ref_axis',(0.0233582592152952,0.209075220419679,0.977620552122803)) ;
#2695 = DIRECTION('',(-0.0233582592152952,-0.209075220419679,-0.977620552122803)) ;
#2696 = DIRECTION('',(0.436264337119824,0.617991140494473,-0.654033927581544)) ;
#2697 = DIRECTION('',(0.459622596335128,0.827066360914232,0.32358662454163)) ;
#2698 = DIRECTION('',(0.0233582592152952,0.209075220419679,0.977620552122803)) ;
#2699 = DIRECTION('',(-0.436264337119824,-0.617991140494473,0.654033927581544)) ;
#2700 = DIRECTION('',(-0.459622596335128,-0.827066360914232,-0.32358662454163)) ;
#2701 = DIRECTION('center_axis',(-0.855521240266964,0.510121382366096,-0.0886542875724541)) ;
#2702 = DIRECTION('ref_axis',(0.0233582592152952,0.209075220419679,0.977620552122803)) ;
#2703 = DIRECTION('',(-0.436264337119824,-0.617991140494473,0.654033927581544)) ;
#2704 = DIRECTION('',(0.0233582592152952,0.209075220419679,0.977620552122803)) ;
#2705 = DIRECTION('',(0.459622596335128,0.827066360914232,0.32358662454163)) ;
#2706 = DIRECTION('',(0.436264337119824,0.617991140494473,-0.654033927581544)) ;
#2707 = DIRECTION('',(-0.0233582592152952,-0.209075220419679,-0.977620552122803)) ;
#2708 = DIRECTION('',(-0.459622596335128,-0.827066360914232,-0.32358662454163)) ;
#2709 = DIRECTION('center_axis',(-0.855521240266964,0.510121382366096,-0.0886542875724541)) ;
#2710 = DIRECTION('ref_axis',(0.517240562193751,0.834304337432909,-0.190783839363105)) ;
#2711 = DIRECTION('center_axis',(-0.51724056219375,-0.83430433743291,0.190783839363105)) ;
#2712 = DIRECTION('ref_axis',(0.0233582592152955,0.209075220419679,0.977620552122803)) ;
#2713 = DIRECTION('',(-0.855521240266964,0.510121382366096,-0.0886542875724541)) ;
#2714 = DIRECTION('',(-0.855521240266964,0.510121382366096,-0.0886542875724541)) ;
#2715 = DIRECTION('center_axis',(-0.51724056219375,-0.83430433743291,0.190783839363105)) ;
#2716 = DIRECTION('ref_axis',(0.0233582592152955,0.209075220419679,0.977620552122803)) ;
#2717 = DIRECTION('',(-0.023358259215295,-0.209075220419679,-0.977620552122803)) ;
#2718 = DIRECTION('center_axis',(-0.51724056219375,-0.83430433743291,0.190783839363105)) ;
#2719 = DIRECTION('ref_axis',(0.0233582592152955,0.209075220419679,0.977620552122803)) ;
#2720 = DIRECTION('',(0.023358259215295,0.209075220419679,0.977620552122803)) ;
#2721 = DIRECTION('center_axis',(0.51724056219375,0.83430433743291,-0.190783839363105)) ;
#2722 = DIRECTION('ref_axis',(0.855521240266964,-0.510121382366095,0.088654287572454)) ;
#2723 = DIRECTION('',(0.51724056219375,0.83430433743291,-0.190783839363105)) ;
#2724 = DIRECTION('',(0.51724056219375,0.83430433743291,-0.190783839363105)) ;
#2725 = DIRECTION('center_axis',(0.51724056219375,0.83430433743291,-0.190783839363105)) ;
#2726 = DIRECTION('ref_axis',(-0.0233582592152955,-0.209075220419679,-0.977620552122803)) ;
#2727 = DIRECTION('center_axis',(0.855521240266964,-0.510121382366096,0.0886542875724541)) ;
#2728 = DIRECTION('ref_axis',(0.0233582592152952,0.209075220419679,0.977620552122803)) ;
#2729 = DIRECTION('',(-0.51724056219375,-0.83430433743291,0.190783839363105)) ;
#2730 = DIRECTION('',(0.0233582592152952,0.209075220419679,0.977620552122803)) ;
#2731 = DIRECTION('center_axis',(-0.855521240266964,0.510121382366096,-0.0886542875724541)) ;
#2732 = DIRECTION('ref_axis',(-0.0233582592152952,-0.209075220419679,-0.977620552122803)) ;
#2733 = DIRECTION('',(-0.51724056219375,-0.83430433743291,0.190783839363105)) ;
#2734 = DIRECTION('',(-0.0233582592152952,-0.209075220419679,-0.977620552122803)) ;
#2735 = DIRECTION('center_axis',(0.51724056219375,0.83430433743291,-0.190783839363105)) ;
#2736 = DIRECTION('ref_axis',(0.0233582592152955,0.209075220419679,0.977620552122803)) ;
#2737 = DIRECTION('center_axis',(0.51724056219375,0.83430433743291,-0.190783839363105)) ;
#2738 = DIRECTION('ref_axis',(-0.0233582592152955,-0.209075220419679,-0.977620552122803)) ;
#2739 = DIRECTION('center_axis',(0.51724056219375,0.83430433743291,-0.190783839363105)) ;
#2740 = DIRECTION('ref_axis',(-0.855521240266964,0.510121382366095,-0.0886542875724542)) ;
#2741 = DIRECTION('center_axis',(-0.238391435228348,-0.236087716531363,0.942036153081598)) ;
#2742 = DIRECTION('ref_axis',(0.459622596335128,0.827066360914232,0.323586624541629)) ;
#2743 = DIRECTION('',(-0.855521240266964,0.510121382366096,-0.0886542875724541)) ;
#2744 = DIRECTION('',(-0.459622596335128,-0.827066360914232,-0.32358662454163)) ;
#2745 = DIRECTION('center_axis',(-0.238391435228348,-0.236087716531363,0.942036153081598)) ;
#2746 = DIRECTION('ref_axis',(-0.855521240266964,0.510121382366096,-0.0886542875724536)) ;
#2747 = DIRECTION('',(0.459622596335128,0.827066360914232,0.32358662454163)) ;
#2748 = DIRECTION('center_axis',(-0.238391435228348,-0.236087716531363,0.942036153081598)) ;
#2749 = DIRECTION('ref_axis',(-0.855521240266964,0.510121382366096,-0.0886542875724536)) ;
#2750 = DIRECTION('center_axis',(-0.278849126965598,-0.598216620901864,-0.75125231371842)) ;
#2751 = DIRECTION('ref_axis',(-0.436264337119824,-0.617991140494473,0.654033927581545)) ;
#2752 = DIRECTION('',(-0.855521240266964,0.510121382366096,-0.0886542875724541)) ;
#2753 = DIRECTION('',(0.436264337119824,0.617991140494473,-0.654033927581544)) ;
#2754 = DIRECTION('center_axis',(-0.278849126965598,-0.598216620901864,-0.75125231371842)) ;
#2755 = DIRECTION('ref_axis',(0.855521240266964,-0.510121382366095,0.0886542875724546)) ;
#2756 = DIRECTION('',(-0.436264337119824,-0.617991140494473,0.654033927581544)) ;
#2757 = DIRECTION('center_axis',(-0.278849126965598,-0.598216620901864,-0.75125231371842)) ;
#2758 = DIRECTION('ref_axis',(0.855521240266964,-0.510121382366095,0.0886542875724546)) ;
#2759 = DIRECTION('center_axis',(0.278849126965598,0.598216620901864,0.75125231371842)) ;
#2760 = DIRECTION('ref_axis',(0.436264337119824,0.617991140494473,-0.654033927581545)) ;
#2761 = DIRECTION('',(-0.855521240266964,0.510121382366096,-0.0886542875724541)) ;
#2762 = DIRECTION('',(-0.436264337119824,-0.617991140494473,0.654033927581544)) ;
#2763 = DIRECTION('center_axis',(0.278849126965598,0.598216620901864,0.75125231371842)) ;
#2764 = DIRECTION('ref_axis',(-0.855521240266964,0.510121382366095,-0.0886542875724546)) ;
#2765 = DIRECTION('',(0.436264337119824,0.617991140494473,-0.654033927581544)) ;
#2766 = DIRECTION('center_axis',(0.278849126965598,0.598216620901864,0.75125231371842)) ;
#2767 = DIRECTION('ref_axis',(-0.855521240266964,0.510121382366095,-0.0886542875724546)) ;
#2768 = DIRECTION('center_axis',(0.238391435228348,0.236087716531363,-0.942036153081598)) ;
#2769 = DIRECTION('ref_axis',(-0.459622596335128,-0.827066360914232,-0.323586624541629)) ;
#2770 = DIRECTION('',(-0.855521240266964,0.510121382366096,-0.0886542875724541)) ;
#2771 = DIRECTION('',(0.459622596335128,0.827066360914232,0.32358662454163)) ;
#2772 = DIRECTION('center_axis',(0.238391435228348,0.236087716531363,-0.942036153081598)) ;
#2773 = DIRECTION('ref_axis',(0.855521240266964,-0.510121382366096,0.0886542875724536)) ;
#2774 = DIRECTION('',(-0.459622596335128,-0.827066360914232,-0.32358662454163)) ;
#2775 = DIRECTION('center_axis',(0.238391435228348,0.236087716531363,-0.942036153081598)) ;
#2776 = DIRECTION('ref_axis',(0.855521240266964,-0.510121382366096,0.0886542875724536)) ;
#2777 = DIRECTION('center_axis',(0.51724056219375,0.83430433743291,-0.190783839363105)) ;
#2778 = DIRECTION('ref_axis',(-0.0233582592152955,-0.209075220419679,-0.977620552122803)) ;
#2779 = DIRECTION('',(0.0233582592152952,0.209075220419679,0.977620552122803)) ;
#2780 = DIRECTION('center_axis',(0.51724056219375,0.83430433743291,-0.190783839363105)) ;
#2781 = DIRECTION('ref_axis',(-0.0233582592152955,-0.209075220419679,-0.977620552122803)) ;
#2782 = DIRECTION('',(-0.0233582592152952,-0.209075220419679,-0.977620552122803)) ;
#2783 = DIRECTION('center_axis',(0.51724056219375,0.83430433743291,-0.190783839363105)) ;
#2784 = DIRECTION('ref_axis',(-0.0233582592152955,-0.209075220419679,-0.977620552122803)) ;
#2785 = DIRECTION('center_axis',(-0.51724056219375,-0.83430433743291,0.190783839363105)) ;
#2786 = DIRECTION('ref_axis',(0.855521240266964,-0.510121382366095,0.088654287572454)) ;
#2787 = DIRECTION('',(-0.51724056219375,-0.83430433743291,0.190783839363105)) ;
#2788 = DIRECTION('',(-0.51724056219375,-0.83430433743291,0.190783839363105)) ;
#2789 = DIRECTION('center_axis',(-0.51724056219375,-0.83430433743291,0.190783839363105)) ;
#2790 = DIRECTION('ref_axis',(0.0233582592152956,0.209075220419679,0.977620552122803)) ;
#2791 = DIRECTION('center_axis',(0.855521240266964,-0.510121382366096,0.0886542875724541)) ;
#2792 = DIRECTION('ref_axis',(0.0233582592152952,0.209075220419679,0.977620552122803)) ;
#2793 = DIRECTION('',(0.51724056219375,0.83430433743291,-0.190783839363105)) ;
#2794 = DIRECTION('',(-0.0233582592152952,-0.209075220419679,-0.977620552122803)) ;
#2795 = DIRECTION('center_axis',(-0.855521240266964,0.510121382366096,-0.0886542875724541)) ;
#2796 = DIRECTION('ref_axis',(-0.0233582592152952,-0.209075220419679,-0.977620552122803)) ;
#2797 = DIRECTION('',(0.51724056219375,0.83430433743291,-0.190783839363105)) ;
#2798 = DIRECTION('',(0.0233582592152952,0.209075220419679,0.977620552122803)) ;
#2799 = DIRECTION('center_axis',(-0.51724056219375,-0.83430433743291,0.190783839363105)) ;
#2800 = DIRECTION('ref_axis',(-0.0233582592152955,-0.209075220419679,-0.977620552122803)) ;
#2801 = DIRECTION('center_axis',(-0.51724056219375,-0.83430433743291,0.190783839363105)) ;
#2802 = DIRECTION('ref_axis',(0.0233582592152956,0.209075220419679,0.977620552122803)) ;
#2803 = DIRECTION('center_axis',(-0.51724056219375,-0.83430433743291,0.190783839363105)) ;
#2804 = DIRECTION('ref_axis',(-0.855521240266964,0.510121382366095,-0.0886542875724539)) ;
#2805 = DIRECTION('center_axis',(0.278849126965598,0.598216620901864,0.75125231371842)) ;
#2806 = DIRECTION('ref_axis',(0.855521240266964,-0.510121382366095,0.0886542875724547)) ;
#2807 = DIRECTION('',(0.278849126965598,0.598216620901864,0.75125231371842)) ;
#2808 = DIRECTION('',(0.278849126965598,0.598216620901864,0.75125231371842)) ;
#2809 = DIRECTION('center_axis',(0.278849126965598,0.598216620901864,0.75125231371842)) ;
#2810 = DIRECTION('ref_axis',(-0.855521240266964,0.510121382366095,-0.0886542875724546)) ;
#2811 = DIRECTION('center_axis',(0.855521240266964,-0.510121382366096,0.0886542875724541)) ;
#2812 = DIRECTION('ref_axis',(0.0233582592152952,0.209075220419679,0.977620552122803)) ;
#2813 = DIRECTION('',(-0.278849126965598,-0.598216620901864,-0.75125231371842)) ;
#2814 = DIRECTION('',(-0.436264337119824,-0.617991140494473,0.654033927581544)) ;
#2815 = DIRECTION('center_axis',(-0.855521240266964,0.510121382366096,-0.0886542875724541)) ;
#2816 = DIRECTION('ref_axis',(-0.0233582592152952,-0.209075220419679,-0.977620552122803)) ;
#2817 = DIRECTION('',(-0.278849126965598,-0.598216620901864,-0.75125231371842)) ;
#2818 = DIRECTION('',(0.436264337119824,0.617991140494473,-0.654033927581544)) ;
#2819 = DIRECTION('center_axis',(0.278849126965598,0.598216620901864,0.75125231371842)) ;
#2820 = DIRECTION('ref_axis',(-0.436264337119824,-0.617991140494473,0.654033927581545)) ;
#2821 = DIRECTION('center_axis',(0.278849126965598,0.598216620901864,0.75125231371842)) ;
#2822 = DIRECTION('ref_axis',(-0.855521240266964,0.510121382366095,-0.0886542875724546)) ;
#2823 = DIRECTION('center_axis',(0.278849126965598,0.598216620901864,0.75125231371842)) ;
#2824 = DIRECTION('ref_axis',(-0.855521240266964,0.510121382366095,-0.0886542875724547)) ;
#2825 = DIRECTION('center_axis',(-0.278849126965598,-0.598216620901864,-0.75125231371842)) ;
#2826 = DIRECTION('ref_axis',(0.855521240266964,-0.510121382366095,0.0886542875724546)) ;
#2827 = DIRECTION('',(-0.278849126965598,-0.598216620901864,-0.75125231371842)) ;
#2828 = DIRECTION('',(-0.278849126965598,-0.598216620901864,-0.75125231371842)) ;
#2829 = DIRECTION('center_axis',(-0.278849126965598,-0.598216620901864,-0.75125231371842)) ;
#2830 = DIRECTION('ref_axis',(0.855521240266964,-0.510121382366095,0.0886542875724546)) ;
#2831 = DIRECTION('center_axis',(0.855521240266964,-0.510121382366096,0.0886542875724541)) ;
#2832 = DIRECTION('ref_axis',(0.0233582592152952,0.209075220419679,0.977620552122803)) ;
#2833 = DIRECTION('',(0.278849126965598,0.598216620901864,0.75125231371842)) ;
#2834 = DIRECTION('',(0.436264337119824,0.617991140494473,-0.654033927581544)) ;
#2835 = DIRECTION('center_axis',(-0.855521240266964,0.510121382366096,-0.0886542875724541)) ;
#2836 = DIRECTION('ref_axis',(-0.0233582592152952,-0.209075220419679,-0.977620552122803)) ;
#2837 = DIRECTION('',(0.278849126965598,0.598216620901864,0.75125231371842)) ;
#2838 = DIRECTION('',(-0.436264337119824,-0.617991140494473,0.654033927581544)) ;
#2839 = DIRECTION('center_axis',(-0.278849126965598,-0.598216620901864,-0.75125231371842)) ;
#2840 = DIRECTION('ref_axis',(0.436264337119824,0.617991140494473,-0.654033927581545)) ;
#2841 = DIRECTION('center_axis',(-0.278849126965598,-0.598216620901864,-0.75125231371842)) ;
#2842 = DIRECTION('ref_axis',(0.855521240266964,-0.510121382366095,0.0886542875724546)) ;
#2843 = DIRECTION('center_axis',(-0.278849126965598,-0.598216620901864,-0.75125231371842)) ;
#2844 = DIRECTION('ref_axis',(-0.855521240266964,0.510121382366095,-0.0886542875724546)) ;
#2845 = DIRECTION('center_axis',(0.238391435228348,0.236087716531363,-0.942036153081598)) ;
#2846 = DIRECTION('ref_axis',(0.855521240266964,-0.510121382366096,0.0886542875724536)) ;
#2847 = DIRECTION('',(0.238391435228348,0.236087716531363,-0.942036153081598)) ;
#2848 = DIRECTION('',(0.238391435228348,0.236087716531363,-0.942036153081598)) ;
#2849 = DIRECTION('center_axis',(0.238391435228348,0.236087716531363,-0.942036153081598)) ;
#2850 = DIRECTION('ref_axis',(0.855521240266964,-0.510121382366096,0.0886542875724536)) ;
#2851 = DIRECTION('center_axis',(0.855521240266964,-0.510121382366096,0.0886542875724541)) ;
#2852 = DIRECTION('ref_axis',(0.0233582592152952,0.209075220419679,0.977620552122803)) ;
#2853 = DIRECTION('',(-0.238391435228348,-0.236087716531363,0.942036153081598)) ;
#2854 = DIRECTION('',(0.459622596335128,0.827066360914232,0.32358662454163)) ;
#2855 = DIRECTION('center_axis',(-0.855521240266964,0.510121382366096,-0.0886542875724541)) ;
#2856 = DIRECTION('ref_axis',(-0.0233582592152952,-0.209075220419679,-0.977620552122803)) ;
#2857 = DIRECTION('',(-0.238391435228348,-0.236087716531363,0.942036153081598)) ;
#2858 = DIRECTION('',(-0.459622596335128,-0.827066360914232,-0.32358662454163)) ;
#2859 = DIRECTION('center_axis',(0.238391435228348,0.236087716531363,-0.942036153081598)) ;
#2860 = DIRECTION('ref_axis',(0.459622596335128,0.827066360914232,0.323586624541629)) ;
#2861 = DIRECTION('center_axis',(0.238391435228348,0.236087716531363,-0.942036153081598)) ;
#2862 = DIRECTION('ref_axis',(0.855521240266964,-0.510121382366096,0.0886542875724536)) ;
#2863 = DIRECTION('center_axis',(0.238391435228348,0.236087716531363,-0.942036153081598)) ;
#2864 = DIRECTION('ref_axis',(-0.855521240266964,0.510121382366096,-0.0886542875724537)) ;
#2865 = DIRECTION('center_axis',(-0.238391435228348,-0.236087716531363,0.942036153081598)) ;
#2866 = DIRECTION('ref_axis',(0.855521240266964,-0.510121382366096,0.0886542875724536)) ;
#2867 = DIRECTION('',(-0.238391435228348,-0.236087716531363,0.942036153081598)) ;
#2868 = DIRECTION('',(-0.238391435228348,-0.236087716531363,0.942036153081598)) ;
#2869 = DIRECTION('center_axis',(-0.238391435228348,-0.236087716531363,0.942036153081598)) ;
#2870 = DIRECTION('ref_axis',(-0.855521240266964,0.510121382366096,-0.0886542875724536)) ;
#2871 = DIRECTION('center_axis',(0.855521240266964,-0.510121382366096,0.0886542875724541)) ;
#2872 = DIRECTION('ref_axis',(0.0233582592152952,0.209075220419679,0.977620552122803)) ;
#2873 = DIRECTION('',(0.238391435228348,0.236087716531363,-0.942036153081598)) ;
#2874 = DIRECTION('',(-0.459622596335128,-0.827066360914232,-0.32358662454163)) ;
#2875 = DIRECTION('center_axis',(-0.855521240266964,0.510121382366096,-0.0886542875724541)) ;
#2876 = DIRECTION('ref_axis',(-0.0233582592152952,-0.209075220419679,-0.977620552122803)) ;
#2877 = DIRECTION('',(0.238391435228348,0.236087716531363,-0.942036153081598)) ;
#2878 = DIRECTION('',(0.459622596335128,0.827066360914232,0.32358662454163)) ;
#2879 = DIRECTION('center_axis',(-0.238391435228348,-0.236087716531363,0.942036153081598)) ;
#2880 = DIRECTION('ref_axis',(-0.459622596335128,-0.827066360914232,-0.323586624541629)) ;
#2881 = DIRECTION('center_axis',(-0.238391435228348,-0.236087716531363,0.942036153081598)) ;
#2882 = DIRECTION('ref_axis',(-0.855521240266964,0.510121382366096,-0.0886542875724536)) ;
#2883 = DIRECTION('center_axis',(-0.238391435228348,-0.236087716531363,0.942036153081598)) ;
#2884 = DIRECTION('ref_axis',(-0.855521240266964,0.510121382366096,-0.0886542875724536)) ;
#2885 = DIRECTION('center_axis',(-0.855521240266964,0.510121382366096,-0.0886542875724541)) ;
#2886 = DIRECTION('ref_axis',(0.0233582592152952,0.209075220419679,0.977620552122803)) ;
#2887 = DIRECTION('center_axis',(-0.855521240266964,0.510121382366096,-0.0886542875724541)) ;
#2888 = DIRECTION('ref_axis',(0.517240562193751,0.834304337432909,-0.190783839363105)) ;
#2889 = DIRECTION('center_axis',(-0.855521240266964,0.510121382366096,-0.0886542875724543)) ;
#2890 = DIRECTION('ref_axis',(-0.509251476733416,-0.798095832523249,0.322034121722927)) ;
#2891 = DIRECTION('center_axis',(-0.093521873895457,-0.320654358089701,-0.942568003775411)) ;
#2892 = DIRECTION('ref_axis',(0.509251476733411,0.798095832523253,-0.322034121722926)) ;
#2893 = DIRECTION('center_axis',(-0.855521240266964,0.510121382366096,-0.0886542875724543)) ;
#2894 = DIRECTION('ref_axis',(0.517240562193751,0.834304337432909,-0.190783839363105)) ;
#2895 = DIRECTION('center_axis',(-0.855521240266964,0.510121382366096,-0.0886542875724543)) ;
#2896 = DIRECTION('ref_axis',(0.517240562193751,0.834304337432909,-0.190783839363105)) ;
#2897 = DIRECTION('center_axis',(-0.855521240266964,0.510121382366096,-0.0886542875724541)) ;
#2898 = DIRECTION('ref_axis',(0.442722751678459,0.631934937682125,-0.636124830267568)) ;
#2899 = DIRECTION('center_axis',(-0.855521240266964,0.510121382366096,-0.0886542875724541)) ;
#2900 = DIRECTION('ref_axis',(0.517240562193751,0.834304337432909,-0.190783839363105)) ;
#2901 = DIRECTION('',(0.855521240266964,-0.510121382366096,0.0886542875724541)) ;
#2902 = DIRECTION('center_axis',(-0.855521240266964,0.510121382366096,-0.0886542875724541)) ;
#2903 = DIRECTION('ref_axis',(0.517240562193751,0.834304337432909,-0.190783839363105)) ;
#2904 = DIRECTION('center_axis',(-0.855521240266964,0.510121382366095,-0.088654287572454)) ;
#2905 = DIRECTION('ref_axis',(0.442722751678459,0.631934937682125,-0.636124830267568)) ;
#2906 = DIRECTION('center_axis',(0.268477136081137,0.583467573897292,0.766476103744976)) ;
#2907 = DIRECTION('ref_axis',(-0.442722751678459,-0.631934937682125,0.636124830267568)) ;
#2908 = DIRECTION('center_axis',(-0.855521240266964,0.510121382366096,-0.0886542875724541)) ;
#2909 = DIRECTION('ref_axis',(0.51724056219375,0.834304337432909,-0.190783839363105)) ;
#2910 = DIRECTION('center_axis',(-0.855521240266964,0.510121382366096,-0.0886542875724541)) ;
#2911 = DIRECTION('ref_axis',(0.51724056219375,0.834304337432909,-0.190783839363105)) ;
#2912 = DIRECTION('center_axis',(-0.855521240266964,0.510121382366096,-0.0886542875724541)) ;
#2913 = DIRECTION('ref_axis',(-0.515977131070524,-0.85419973905181,0.06411244821445)) ;
#2914 = DIRECTION('center_axis',(-0.0430233386001843,0.100593146171714,0.99399698756031)) ;
#2915 = DIRECTION('ref_axis',(0.515977131070522,0.854199739051811,-0.0641124482144504)) ;
#2916 = DIRECTION('axis',(0.,0.,1.)) ;
#2917 = DIRECTION('refdir',(1.,0.,0.)) ;
#2918 = DIRECTION('center_axis',(0.855521240266964,-0.510121382366096,0.0886542875724545)) ;
#2919 = DIRECTION('ref_axis',(-0.465119843688758,-0.83240693799912,-0.301267689236459)) ;
#2920 = DIRECTION('center_axis',(0.855521240266964,-0.510121382366096,0.0886542875724545)) ;
#2921 = DIRECTION('ref_axis',(-0.517240562193751,-0.834304337432909,0.190783839363105)) ;
#2922 = DIRECTION('',(-0.855521240266964,0.510121382366096,-0.0886542875724545)) ;
#2923 = DIRECTION('center_axis',(0.855521240266964,-0.510121382366096,0.0886542875724545)) ;
#2924 = DIRECTION('ref_axis',(-0.517240562193751,-0.834304337432909,0.190783839363105)) ;
#2925 = DIRECTION('center_axis',(0.855521240266964,-0.510121382366096,0.0886542875724545)) ;
#2926 = DIRECTION('ref_axis',(-0.465119843688758,-0.83240693799912,-0.301267689236459)) ;
#2927 = DIRECTION('center_axis',(0.855521240266964,-0.510121382366096,0.0886542875724545)) ;
#2928 = DIRECTION('ref_axis',(-0.517240562193751,-0.834304337432909,0.190783839363105)) ;
#2929 = DIRECTION('',(-0.855521240266964,0.510121382366096,-0.0886542875724545)) ;
#2930 = DIRECTION('center_axis',(0.855521240266964,-0.510121382366096,0.0886542875724545)) ;
#2931 = DIRECTION('ref_axis',(-0.517240562193751,-0.834304337432909,0.190783839363105)) ;
#2932 = DIRECTION('center_axis',(-0.855521240266964,0.510121382366096,-0.0886542875724545)) ;
#2933 = DIRECTION('ref_axis',(-0.465119843688757,-0.83240693799912,-0.301267689236459)) ;
#2934 = DIRECTION('',(0.472058877340417,-0.877268648914429,-0.0869490307936615)) ;
#2935 = DIRECTION('center_axis',(-0.855521240266964,0.510121382366096,-0.0886542875724545)) ;
#2936 = DIRECTION('ref_axis',(0.517240562193751,0.834304337432909,-0.190783839363105)) ;
#2937 = DIRECTION('center_axis',(0.855521240266964,-0.510121382366096,0.0886542875724545)) ;
#2938 = DIRECTION('ref_axis',(-0.465119843688757,-0.83240693799912,-0.301267689236459)) ;
#2939 = DIRECTION('center_axis',(0.855521240266964,-0.510121382366096,0.0886542875724545)) ;
#2940 = DIRECTION('ref_axis',(-0.517240562193751,-0.834304337432909,0.190783839363105)) ;
#2941 = DIRECTION('',(-0.855521240266964,0.510121382366096,-0.0886542875724545)) ;
#2942 = DIRECTION('center_axis',(-0.855521240266964,0.510121382366096,-0.0886542875724545)) ;
#2943 = DIRECTION('ref_axis',(-0.465119843688757,-0.83240693799912,-0.301267689236459)) ;
#2944 = DIRECTION('',(0.276055474905567,-0.949310879265127,-0.150340378087633)) ;
#2945 = DIRECTION('center_axis',(-0.855521240266964,0.510121382366096,-0.0886542875724545)) ;
#2946 = DIRECTION('ref_axis',(0.51724056219375,0.834304337432909,-0.190783839363105)) ;
#2947 = DIRECTION('center_axis',(0.855521240266964,-0.510121382366096,0.0886542875724545)) ;
#2948 = DIRECTION('ref_axis',(-0.465119843688758,-0.83240693799912,-0.301267689236459)) ;
#2949 = DIRECTION('center_axis',(0.855521240266964,-0.510121382366096,0.0886542875724545)) ;
#2950 = DIRECTION('ref_axis',(-0.517240562193751,-0.834304337432909,0.190783839363105)) ;
#2951 = DIRECTION('',(0.933834265978767,0.22789030186616,0.275716473935179)) ;
#2952 = DIRECTION('center_axis',(0.855521240266964,-0.510121382366096,0.0886542875724545)) ;
#2953 = DIRECTION('ref_axis',(-0.517240562193751,-0.834304337432909,0.190783839363105)) ;
#2954 = DIRECTION('center_axis',(0.855521240266964,-0.510121382366096,0.0886542875724545)) ;
#2955 = DIRECTION('ref_axis',(-0.465119843688758,-0.83240693799912,-0.301267689236459)) ;
#2956 = DIRECTION('center_axis',(0.855521240266964,-0.510121382366096,0.0886542875724545)) ;
#2957 = DIRECTION('ref_axis',(-0.517240562193751,-0.834304337432909,0.190783839363105)) ;
#2958 = DIRECTION('',(0.855521240266964,-0.510121382366096,0.0886542875724545)) ;
#2959 = DIRECTION('center_axis',(-0.855521240266964,0.510121382366096,-0.0886542875724545)) ;
#2960 = DIRECTION('ref_axis',(-0.465119843688758,-0.83240693799912,-0.301267689236459)) ;
#2961 = DIRECTION('',(-0.434020190478197,0.895315978292129,0.100178706679998)) ;
#2962 = DIRECTION('center_axis',(-0.855521240266964,0.510121382366096,-0.0886542875724545)) ;
#2963 = DIRECTION('ref_axis',(0.517240562193751,0.834304337432909,-0.190783839363105)) ;
#2964 = DIRECTION('center_axis',(0.855521240266964,-0.510121382366096,0.0886542875724545)) ;
#2965 = DIRECTION('ref_axis',(-0.465119843688757,-0.83240693799912,-0.301267689236459)) ;
#2966 = DIRECTION('center_axis',(0.855521240266964,-0.510121382366096,0.0886542875724545)) ;
#2967 = DIRECTION('ref_axis',(-0.517240562193751,-0.834304337432909,0.190783839363105)) ;
#2968 = DIRECTION('',(0.855521240266964,-0.510121382366096,0.0886542875724545)) ;
#2969 = DIRECTION('center_axis',(0.855521240266964,-0.510121382366096,0.0886542875724545)) ;
#2970 = DIRECTION('ref_axis',(-0.465119843688758,-0.83240693799912,-0.301267689236459)) ;
#2971 = DIRECTION('center_axis',(0.855521240266964,-0.510121382366096,0.0886542875724545)) ;
#2972 = DIRECTION('ref_axis',(-0.517240562193751,-0.834304337432909,0.190783839363105)) ;
#2973 = DIRECTION('',(0.830566220570463,0.465824863413527,0.305232616004688)) ;
#2974 = DIRECTION('center_axis',(0.855521240266964,-0.510121382366096,0.0886542875724545)) ;
#2975 = DIRECTION('ref_axis',(-0.517240562193751,-0.834304337432909,0.190783839363105)) ;
#2976 = DIRECTION('center_axis',(0.855521240266964,-0.510121382366096,0.0886542875724545)) ;
#2977 = DIRECTION('ref_axis',(-0.465119843688758,-0.83240693799912,-0.301267689236459)) ;
#2978 = DIRECTION('center_axis',(0.855521240266964,-0.510121382366096,0.0886542875724545)) ;
#2979 = DIRECTION('ref_axis',(-0.517240562193751,-0.834304337432909,0.190783839363105)) ;
#2980 = DIRECTION('',(0.855521240266964,-0.510121382366096,0.0886542875724545)) ;
#2981 = DIRECTION('center_axis',(-0.855521240266964,0.510121382366096,-0.0886542875724545)) ;
#2982 = DIRECTION('ref_axis',(-0.465119843688758,-0.83240693799912,-0.301267689236459)) ;
#2983 = DIRECTION('',(-0.0249550196914587,0.975946245776617,0.216578328432755)) ;
#2984 = DIRECTION('center_axis',(-0.855521240266964,0.510121382366096,-0.0886542875724545)) ;
#2985 = DIRECTION('ref_axis',(0.517240562193751,0.834304337432909,-0.190783839363105)) ;
#2986 = DIRECTION('center_axis',(0.855521240266964,-0.510121382366096,0.0886542875724545)) ;
#2987 = DIRECTION('ref_axis',(-0.465119843688757,-0.83240693799912,-0.301267689236459)) ;
#2988 = DIRECTION('center_axis',(0.855521240266964,-0.510121382366096,0.0886542875724545)) ;
#2989 = DIRECTION('ref_axis',(-0.517240562193751,-0.834304337432909,0.190783839363105)) ;
#2990 = DIRECTION('',(0.855521240266964,-0.510121382366096,0.0886542875724545)) ;
#2991 = DIRECTION('center_axis',(-0.855521240266964,0.510121382366096,-0.0886542875724545)) ;
#2992 = DIRECTION('ref_axis',(-0.465119843688757,-0.83240693799912,-0.301267689236459)) ;
#2993 = DIRECTION('',(-0.276055474905567,0.949310879265127,0.150340378087633)) ;
#2994 = DIRECTION('center_axis',(-0.855521240266964,0.510121382366096,-0.0886542875724545)) ;
#2995 = DIRECTION('ref_axis',(0.517240562193751,0.834304337432909,-0.190783839363105)) ;
#2996 = DIRECTION('center_axis',(0.855521240266964,-0.510121382366096,0.0886542875724545)) ;
#2997 = DIRECTION('ref_axis',(0.0233582592152947,0.209075220419679,0.977620552122803)) ;
#2998 = DIRECTION('center_axis',(0.855521240266964,-0.510121382366096,0.0886542875724545)) ;
#2999 = DIRECTION('ref_axis',(0.0233582592152947,0.209075220419679,0.977620552122803)) ;
#3000 = DIRECTION('center_axis',(0.855521240266964,-0.510121382366096,0.0886542875724545)) ;
#3001 = DIRECTION('ref_axis',(0.0233582592152947,0.209075220419679,0.977620552122803)) ;
#3002 = DIRECTION('center_axis',(0.855521240266964,-0.510121382366096,0.0886542875724545)) ;
#3003 = DIRECTION('ref_axis',(0.0233582592152947,0.209075220419679,0.977620552122803)) ;
#3004 = DIRECTION('center_axis',(0.855521240266964,-0.510121382366096,0.0886542875724545)) ;
#3005 = DIRECTION('ref_axis',(-0.227479534154222,-0.216506038769899,0.949409393632244)) ;
#3006 = DIRECTION('center_axis',(0.855521240266964,-0.510121382366096,0.0886542875724545)) ;
#3007 = DIRECTION('ref_axis',(-0.517240562193751,-0.834304337432909,0.190783839363105)) ;
#3008 = DIRECTION('',(0.855521240266964,-0.510121382366096,0.0886542875724545)) ;
#3009 = DIRECTION('center_axis',(0.855521240266964,-0.510121382366096,0.0886542875724545)) ;
#3010 = DIRECTION('ref_axis',(-0.465119843688758,-0.83240693799912,-0.301267689236459)) ;
#3011 = DIRECTION('center_axis',(0.855521240266964,-0.510121382366096,0.0886542875724545)) ;
#3012 = DIRECTION('ref_axis',(-0.517240562193751,-0.834304337432909,0.190783839363105)) ;
#3013 = DIRECTION('',(-0.855521240266964,0.510121382366096,-0.0886542875724545)) ;
#3014 = DIRECTION('center_axis',(0.855521240266964,-0.510121382366096,0.0886542875724545)) ;
#3015 = DIRECTION('ref_axis',(-0.517240562193751,-0.834304337432909,0.190783839363105)) ;
#3016 = DIRECTION('center_axis',(0.855521240266964,-0.510121382366096,0.0886542875724545)) ;
#3017 = DIRECTION('ref_axis',(0.0233582592152947,0.209075220419679,0.977620552122803)) ;
#3018 = DIRECTION('center_axis',(0.855521240266964,-0.510121382366096,0.0886542875724545)) ;
#3019 = DIRECTION('ref_axis',(-0.517240562193751,-0.834304337432909,0.190783839363105)) ;
#3020 = DIRECTION('center_axis',(-0.855521240266964,0.510121382366096,-0.0886542875724545)) ;
#3021 = DIRECTION('ref_axis',(-0.465119843688758,-0.83240693799912,-0.301267689236459)) ;
#3022 = DIRECTION('center_axis',(-0.855521240266964,0.510121382366096,-0.0886542875724545)) ;
#3023 = DIRECTION('ref_axis',(0.517240562193751,0.834304337432909,-0.190783839363105)) ;
#3024 = DIRECTION('',(-0.276055474905567,0.949310879265127,0.150340378087633)) ;
#3025 = DIRECTION('center_axis',(0.855521240266964,-0.510121382366096,0.0886542875724545)) ;
#3026 = DIRECTION('ref_axis',(-0.465119843688758,-0.83240693799912,-0.301267689236459)) ;
#3027 = DIRECTION('',(0.855521240266964,-0.510121382366096,0.0886542875724545)) ;
#3028 = DIRECTION('center_axis',(0.855521240266964,-0.510121382366096,0.0886542875724545)) ;
#3029 = DIRECTION('ref_axis',(-0.517240562193751,-0.834304337432909,0.190783839363105)) ;
#3030 = DIRECTION('center_axis',(0.855521240266964,-0.510121382366096,0.0886542875724545)) ;
#3031 = DIRECTION('ref_axis',(0.0233582592152947,0.209075220419679,0.977620552122803)) ;
#3032 = DIRECTION('center_axis',(0.855521240266964,-0.510121382366096,0.0886542875724545)) ;
#3033 = DIRECTION('ref_axis',(-0.517240562193751,-0.834304337432909,0.190783839363105)) ;
#3034 = DIRECTION('center_axis',(0.855521240266964,-0.510121382366096,0.0886542875724545)) ;
#3035 = DIRECTION('ref_axis',(-0.465119843688758,-0.83240693799912,-0.301267689236459)) ;
#3036 = DIRECTION('',(-0.855521240266964,0.510121382366096,-0.0886542875724545)) ;
#3037 = DIRECTION('center_axis',(0.855521240266964,-0.510121382366096,0.0886542875724545)) ;
#3038 = DIRECTION('ref_axis',(-0.517240562193751,-0.834304337432909,0.190783839363105)) ;
#3039 = DIRECTION('center_axis',(0.855521240266964,-0.510121382366096,0.0886542875724545)) ;
#3040 = DIRECTION('ref_axis',(-0.465119843688758,-0.83240693799912,-0.301267689236459)) ;
#3041 = DIRECTION('center_axis',(0.855521240266964,-0.510121382366096,0.0886542875724545)) ;
#3042 = DIRECTION('ref_axis',(-0.517240562193751,-0.834304337432909,0.190783839363105)) ;
#3043 = DIRECTION('',(-0.855521240266964,0.510121382366096,-0.0886542875724545)) ;
#3044 = DIRECTION('center_axis',(0.855521240266964,-0.510121382366096,0.0886542875724545)) ;
#3045 = DIRECTION('ref_axis',(-0.517240562193751,-0.834304337432909,0.190783839363105)) ;
#3046 = DIRECTION('center_axis',(0.855521240266964,-0.510121382366096,0.0886542875724545)) ;
#3047 = DIRECTION('ref_axis',(0.0233582592152947,0.209075220419679,0.977620552122803)) ;
#3048 = DIRECTION('center_axis',(0.855521240266964,-0.510121382366096,0.0886542875724545)) ;
#3049 = DIRECTION('ref_axis',(-0.517240562193751,-0.834304337432909,0.190783839363105)) ;
#3050 = DIRECTION('center_axis',(0.855521240266964,-0.510121382366096,0.0886542875724545)) ;
#3051 = DIRECTION('ref_axis',(-0.465119843688757,-0.83240693799912,-0.301267689236459)) ;
#3052 = DIRECTION('',(-0.855521240266964,0.510121382366096,-0.0886542875724545)) ;
#3053 = DIRECTION('center_axis',(0.855521240266964,-0.510121382366096,0.0886542875724545)) ;
#3054 = DIRECTION('ref_axis',(-0.517240562193751,-0.834304337432909,0.190783839363105)) ;
#3055 = DIRECTION('center_axis',(0.855521240266964,-0.510121382366096,0.0886542875724545)) ;
#3056 = DIRECTION('ref_axis',(0.0233582592152947,0.209075220419679,0.977620552122803)) ;
#3057 = DIRECTION('center_axis',(0.855521240266964,-0.510121382366096,0.0886542875724545)) ;
#3058 = DIRECTION('ref_axis',(-0.517240562193751,-0.834304337432909,0.190783839363105)) ;
#3059 = DIRECTION('center_axis',(0.855521240266964,-0.510121382366096,0.0886542875724545)) ;
#3060 = DIRECTION('ref_axis',(-0.465119843688758,-0.83240693799912,-0.301267689236459)) ;
#3061 = DIRECTION('',(-0.855521240266964,0.510121382366096,-0.0886542875724545)) ;
#3062 = DIRECTION('center_axis',(0.855521240266964,-0.510121382366096,0.0886542875724545)) ;
#3063 = DIRECTION('ref_axis',(-0.517240562193751,-0.834304337432909,0.190783839363105)) ;
#3064 = DIRECTION('center_axis',(0.855521240266964,-0.510121382366096,0.0886542875724545)) ;
#3065 = DIRECTION('ref_axis',(0.0233582592152947,0.209075220419679,0.977620552122803)) ;
#3066 = DIRECTION('center_axis',(0.855521240266964,-0.510121382366096,0.0886542875724545)) ;
#3067 = DIRECTION('ref_axis',(-0.517240562193751,-0.834304337432909,0.190783839363105)) ;
#3068 = DIRECTION('center_axis',(0.855521240266964,-0.510121382366096,0.0886542875724545)) ;
#3069 = DIRECTION('ref_axis',(-0.517240562193751,-0.834304337432909,0.190783839363105)) ;
#3070 = DIRECTION('center_axis',(-0.855521240266964,0.510121382366096,-0.0886542875724545)) ;
#3071 = DIRECTION('ref_axis',(-0.465119843688758,-0.83240693799912,-0.301267689236459)) ;
#3072 = DIRECTION('',(0.220742469906792,-0.961054902255409,-0.166271575533209)) ;
#3073 = DIRECTION('center_axis',(0.855521240266964,-0.510121382366096,0.0886542875724545)) ;
#3074 = DIRECTION('ref_axis',(-0.289065833361634,-0.612632535208754,-0.735610169034278)) ;
#3075 = DIRECTION('',(0.855521240266964,-0.510121382366096,0.0886542875724545)) ;
#3076 = DIRECTION('center_axis',(0.855521240266964,-0.510121382366096,0.0886542875724545)) ;
#3077 = DIRECTION('ref_axis',(0.516545367515822,0.829138573978605,-0.213799224597913)) ;
#3078 = DIRECTION('',(0.855521240266964,-0.510121382366096,0.0886542875724545)) ;
#3079 = DIRECTION('center_axis',(0.855521240266964,-0.510121382366096,0.0886542875724545)) ;
#3080 = DIRECTION('ref_axis',(0.0233582592152947,0.209075220419679,0.977620552122803)) ;
#3081 = DIRECTION('center_axis',(0.855521240266964,-0.510121382366096,0.0886542875724545)) ;
#3082 = DIRECTION('ref_axis',(-0.517240562193751,-0.834304337432909,0.190783839363105)) ;
#3083 = DIRECTION('center_axis',(0.855521240266964,-0.510121382366096,0.0886542875724545)) ;
#3084 = DIRECTION('ref_axis',(-0.517240562193751,-0.834304337432909,0.190783839363105)) ;
#3085 = DIRECTION('center_axis',(0.855521240266964,-0.510121382366096,0.0886542875724545)) ;
#3086 = DIRECTION('ref_axis',(0.0233582592152947,0.209075220419679,0.977620552122803)) ;
#3087 = DIRECTION('center_axis',(0.855521240266964,-0.510121382366096,0.0886542875724545)) ;
#3088 = DIRECTION('ref_axis',(-0.517240562193751,-0.834304337432909,0.190783839363105)) ;
#3089 = DIRECTION('center_axis',(0.855521240266964,-0.510121382366096,0.0886542875724545)) ;
#3090 = DIRECTION('ref_axis',(-0.517240562193751,-0.834304337432909,0.190783839363105)) ;
#3091 = DIRECTION('center_axis',(0.855521240266964,-0.510121382366096,0.0886542875724545)) ;
#3092 = DIRECTION('ref_axis',(-0.465119843688758,-0.83240693799912,-0.301267689236459)) ;
#3093 = DIRECTION('center_axis',(0.855521240266964,-0.510121382366096,0.0886542875724545)) ;
#3094 = DIRECTION('ref_axis',(-0.517240562193751,-0.834304337432909,0.190783839363105)) ;
#3095 = DIRECTION('center_axis',(0.855521240266964,-0.510121382366096,0.0886542875724545)) ;
#3096 = DIRECTION('ref_axis',(-0.517240562193751,-0.834304337432909,0.190783839363105)) ;
#3097 = DIRECTION('',(0.855521240266964,-0.510121382366096,0.0886542875724545)) ;
#3098 = DIRECTION('center_axis',(-0.22747999965104,-0.216506928060168,0.949409079301811)) ;
#3099 = DIRECTION('ref_axis',(0.421816601389418,0.856842394307428,0.296465623824745)) ;
#3100 = DIRECTION('center_axis',(0.227479534082472,0.216506038642441,-0.949409393678501)) ;
#3101 = DIRECTION('ref_axis',(-0.507262223798798,-0.805894130045609,-0.305318992964293)) ;
#3102 = DIRECTION('center_axis',(-0.855521239991043,0.510121383082549,-0.088654286112606)) ;
#3103 = DIRECTION('ref_axis',(-0.46511984467153,-0.832406937392223,-0.301267689396044)) ;
#3104 = DIRECTION('center_axis',(0.855521240266964,-0.510121382366096,0.0886542875724545)) ;
#3105 = DIRECTION('ref_axis',(-0.465119843688758,-0.83240693799912,-0.301267689236459)) ;
#3106 = DIRECTION('center_axis',(0.855521240266964,-0.510121382366096,0.0886542875724545)) ;
#3107 = DIRECTION('ref_axis',(-0.517240562193751,-0.834304337432909,0.190783839363105)) ;
#3108 = DIRECTION('',(-0.855521240266964,0.510121382366096,-0.0886542875724545)) ;
#3109 = DIRECTION('center_axis',(0.855521240266964,-0.510121382366096,0.0886542875724545)) ;
#3110 = DIRECTION('ref_axis',(-0.517240562193751,-0.834304337432909,0.190783839363105)) ;
#3111 = DIRECTION('center_axis',(0.855521240266964,-0.510121382366096,0.0886542875724545)) ;
#3112 = DIRECTION('ref_axis',(0.509998973339437,0.80069041569811,-0.314318159516608)) ;
#3113 = DIRECTION('center_axis',(0.855521240266964,-0.510121382366096,0.0886542875724545)) ;
#3114 = DIRECTION('ref_axis',(-0.517240562193751,-0.834304337432909,0.190783839363105)) ;
#3115 = DIRECTION('center_axis',(0.0893557756655708,0.314119457312169,0.945169038793121)) ;
#3116 = DIRECTION('ref_axis',(-0.509998973339439,-0.800690415698109,0.314318159516608)) ;
#3117 = DIRECTION('center_axis',(0.855521240266964,-0.510121382366096,0.0886542875724545)) ;
#3118 = DIRECTION('ref_axis',(-0.517240562193751,-0.834304337432909,0.190783839363105)) ;
#3119 = DIRECTION('center_axis',(0.855521240266964,-0.510121382366096,0.0886542875724545)) ;
#3120 = DIRECTION('ref_axis',(-0.465119843688757,-0.832406937999119,-0.301267689236459)) ;
#3121 = DIRECTION('',(-0.855521240266964,0.510121382366096,-0.0886542875724545)) ;
#3122 = DIRECTION('center_axis',(0.855521240266964,-0.510121382366096,0.0886542875724545)) ;
#3123 = DIRECTION('ref_axis',(-0.517240562193751,-0.834304337432909,0.190783839363105)) ;
#3124 = DIRECTION('center_axis',(0.855521240266964,-0.510121382366096,0.0886542875724545)) ;
#3125 = DIRECTION('ref_axis',(-0.517240562193751,-0.834304337432909,0.190783839363105)) ;
#3126 = DIRECTION('center_axis',(0.855521240266964,-0.510121382366096,0.0886542875724545)) ;
#3127 = DIRECTION('ref_axis',(-0.465119843688758,-0.83240693799912,-0.301267689236459)) ;
#3128 = DIRECTION('center_axis',(0.855521240266964,-0.510121382366096,0.0886542875724545)) ;
#3129 = DIRECTION('ref_axis',(-0.517240562193751,-0.834304337432909,0.190783839363105)) ;
#3130 = DIRECTION('center_axis',(0.855521240266964,-0.510121382366096,0.0886542875724545)) ;
#3131 = DIRECTION('ref_axis',(-0.517240562193751,-0.834304337432909,0.190783839363105)) ;
#3132 = DIRECTION('',(-0.877680816263419,0.467916504938536,-0.103588267527187)) ;
#3133 = DIRECTION('center_axis',(0.227477963935797,0.216503188953687,-0.94941041973243)) ;
#3134 = DIRECTION('ref_axis',(0.465119508114888,0.832408339490032,0.301264334959204)) ;
#3135 = DIRECTION('center_axis',(-0.227479533901985,-0.216506038339706,0.949409393790783)) ;
#3136 = DIRECTION('ref_axis',(-0.465119843754982,-0.832406938143867,-0.301267688734278)) ;
#3137 = DIRECTION('center_axis',(0.855521240266964,-0.510121382366096,0.0886542875724545)) ;
#3138 = DIRECTION('ref_axis',(-0.465119843688758,-0.83240693799912,-0.301267689236459)) ;
#3139 = DIRECTION('',(0.855521240266964,-0.510121382366096,0.0886542875724545)) ;
#3140 = DIRECTION('center_axis',(0.855521240266964,-0.510121382366096,0.0886542875724545)) ;
#3141 = DIRECTION('ref_axis',(-0.517240562193751,-0.834304337432909,0.190783839363105)) ;
#3142 = DIRECTION('center_axis',(0.855521240266964,-0.510121382366096,0.0886542875724545)) ;
#3143 = DIRECTION('ref_axis',(-0.465119843688758,-0.83240693799912,-0.301267689236459)) ;
#3144 = DIRECTION('center_axis',(0.855521240266964,-0.510121382366096,0.0886542875724545)) ;
#3145 = DIRECTION('ref_axis',(-0.517240562193751,-0.834304337432909,0.190783839363105)) ;
#3146 = DIRECTION('',(0.877680816263419,-0.467916504938536,0.103588267527187)) ;
#3147 = DIRECTION('center_axis',(-0.855521240266964,0.510121382366096,-0.0886542875724545)) ;
#3148 = DIRECTION('ref_axis',(-0.465119843688759,-0.83240693799912,-0.301267689236457)) ;
#3149 = DIRECTION('center_axis',(0.227479534154222,0.216506038769899,-0.949409393632244)) ;
#3150 = DIRECTION('ref_axis',(0.465119843688757,0.83240693799912,0.301267689236458)) ;
#3151 = DIRECTION('axis',(0.,0.,1.)) ;
#3152 = DIRECTION('refdir',(1.,0.,0.)) ;
#3153 = DIRECTION('center_axis',(0.,-1.,0.)) ;
#3154 = DIRECTION('ref_axis',(-0.479425538604203,0.,0.877582561890373)) ;
#3155 = DIRECTION('center_axis',(0.,-1.,0.)) ;
#3156 = DIRECTION('ref_axis',(0.,0.,1.)) ;
#3157 = DIRECTION('',(0.,-1.,0.)) ;
#3158 = DIRECTION('center_axis',(0.,-1.,0.)) ;
#3159 = DIRECTION('ref_axis',(0.,0.,1.)) ;
#3160 = DIRECTION('center_axis',(0.,-1.,0.)) ;
#3161 = DIRECTION('ref_axis',(-0.479425538604204,0.,0.877582561890372)) ;
#3162 = DIRECTION('center_axis',(0.,-1.,0.)) ;
#3163 = DIRECTION('ref_axis',(0.,0.,1.)) ;
#3164 = DIRECTION('',(0.339005049420894,-0.707106781186865,-0.620544580563467)) ;
#3165 = DIRECTION('center_axis',(0.,-1.,0.)) ;
#3166 = DIRECTION('ref_axis',(-0.479425538604204,0.,0.877582561890372)) ;
#3167 = DIRECTION('center_axis',(0.,-1.,0.)) ;
#3168 = DIRECTION('ref_axis',(0.,0.,1.)) ;
#3169 = DIRECTION('',(0.,-1.,0.)) ;
#3170 = DIRECTION('center_axis',(0.,1.,0.)) ;
#3171 = DIRECTION('ref_axis',(-0.479425538604204,0.,0.877582561890372)) ;
#3172 = DIRECTION('',(0.339005049420894,0.707106781186865,-0.620544580563467)) ;
#3173 = DIRECTION('center_axis',(0.,1.,0.)) ;
#3174 = DIRECTION('ref_axis',(0.,0.,-1.)) ;
#3175 = DIRECTION('center_axis',(-8.80690426921701E-17,-1.,1.61209301310987E-16)) ;
#3176 = DIRECTION('ref_axis',(-0.479425538604204,1.22464679914735E-16,0.877582561890372)) ;
#3177 = DIRECTION('center_axis',(0.,-1.,0.)) ;
#3178 = DIRECTION('ref_axis',(0.,0.,1.)) ;
#3179 = DIRECTION('center_axis',(-0.877582561890372,-1.42222518970134E-31,
-0.479425538604204)) ;
#3180 = DIRECTION('ref_axis',(0.479425538604204,-1.22464679914735E-16,-0.877582561890372)) ;
#3181 = DIRECTION('center_axis',(0.,-1.,0.)) ;
#3182 = DIRECTION('ref_axis',(1.,0.,0.)) ;
#3183 = DIRECTION('center_axis',(0.,-1.,0.)) ;
#3184 = DIRECTION('ref_axis',(0.,0.,1.)) ;
#3185 = DIRECTION('center_axis',(0.,-1.,0.)) ;
#3186 = DIRECTION('ref_axis',(0.136069885869001,0.,-0.990699241021006)) ;
#3187 = DIRECTION('center_axis',(-0.990699241021006,0.,-0.136069885869001)) ;
#3188 = DIRECTION('ref_axis',(-0.136069885869001,0.,0.990699241021006)) ;
#3189 = DIRECTION('center_axis',(0.,-1.,0.)) ;
#3190 = DIRECTION('ref_axis',(0.,0.,1.)) ;
#3191 = DIRECTION('center_axis',(0.,-1.,0.)) ;
#3192 = DIRECTION('ref_axis',(0.,0.,1.)) ;
#3193 = DIRECTION('center_axis',(-8.80690426921701E-17,-1.,1.61209301310987E-16)) ;
#3194 = DIRECTION('ref_axis',(-0.479425538604204,0.,0.877582561890372)) ;
#3195 = DIRECTION('center_axis',(0.877582561890372,1.42222518970134E-31,0.479425538604204)) ;
#3196 = DIRECTION('ref_axis',(0.479425538604204,0.,-0.877582561890372)) ;
#3197 = DIRECTION('center_axis',(0.,-1.,0.)) ;
#3198 = DIRECTION('ref_axis',(0.,0.,1.)) ;
#3199 = DIRECTION('center_axis',(0.,-1.,0.)) ;
#3200 = DIRECTION('ref_axis',(0.,0.,1.)) ;
#3201 = DIRECTION('center_axis',(0.,-1.,0.)) ;
#3202 = DIRECTION('ref_axis',(-0.127966679280044,0.,-0.991778467700342)) ;
#3203 = DIRECTION('center_axis',(0.991778467700342,0.,-0.127966679280044)) ;
#3204 = DIRECTION('ref_axis',(0.127966679280044,0.,0.991778467700342)) ;
#3205 = DIRECTION('center_axis',(0.,-1.,0.)) ;
#3206 = DIRECTION('ref_axis',(0.,0.,1.)) ;
#3207 = DIRECTION('center_axis',(0.,-1.,0.)) ;
#3208 = DIRECTION('ref_axis',(0.,0.,1.)) ;
#3209 = DIRECTION('center_axis',(0.,-1.,0.)) ;
#3210 = DIRECTION('ref_axis',(-0.479425538604204,0.,0.877582561890372)) ;
#3211 = DIRECTION('',(0.,1.,0.)) ;
#3212 = DIRECTION('center_axis',(0.,-1.,0.)) ;
#3213 = DIRECTION('ref_axis',(0.,0.,1.)) ;
#3214 = DIRECTION('center_axis',(0.,-1.,0.)) ;
#3215 = DIRECTION('ref_axis',(0.,0.,1.)) ;
#3216 = DIRECTION('center_axis',(0.,-1.,0.)) ;
#3217 = DIRECTION('ref_axis',(-0.127966679280044,0.,-0.991778467700342)) ;
#3218 = DIRECTION('center_axis',(0.991778467700342,0.,-0.127966679280044)) ;
#3219 = DIRECTION('ref_axis',(0.127966679280044,0.,0.991778467700342)) ;
#3220 = DIRECTION('center_axis',(0.,-1.,0.)) ;
#3221 = DIRECTION('ref_axis',(0.,0.,1.)) ;
#3222 = DIRECTION('center_axis',(0.,-1.,0.)) ;
#3223 = DIRECTION('ref_axis',(0.,0.,1.)) ;
#3224 = DIRECTION('center_axis',(0.,-1.,0.)) ;
#3225 = DIRECTION('ref_axis',(0.405193516143217,0.,-0.91423094154349)) ;
#3226 = DIRECTION('center_axis',(0.,-1.,0.)) ;
#3227 = DIRECTION('ref_axis',(0.,0.,1.)) ;
#3228 = DIRECTION('center_axis',(0.,-1.,0.)) ;
#3229 = DIRECTION('ref_axis',(0.,0.,1.)) ;
#3230 = DIRECTION('center_axis',(-0.91423094154349,0.,-0.405193516143217)) ;
#3231 = DIRECTION('ref_axis',(-0.405193516143217,0.,0.91423094154349)) ;
#3232 = DIRECTION('center_axis',(0.,-1.,0.)) ;
#3233 = DIRECTION('ref_axis',(0.,0.,1.)) ;
#3234 = DIRECTION('center_axis',(0.,1.,0.)) ;
#3235 = DIRECTION('ref_axis',(-0.479425538604204,0.,0.877582561890372)) ;
#3236 = DIRECTION('center_axis',(0.,1.,0.)) ;
#3237 = DIRECTION('ref_axis',(0.,0.,-1.)) ;
#3238 = DIRECTION('',(-0.165739977854205,-0.938343116817079,0.303384994459016)) ;
#3239 = DIRECTION('center_axis',(0.,-1.,0.)) ;
#3240 = DIRECTION('ref_axis',(-0.479425538604203,0.,0.877582561890373)) ;
#3241 = DIRECTION('center_axis',(0.,-1.,0.)) ;
#3242 = DIRECTION('ref_axis',(0.,0.,1.)) ;
#3243 = DIRECTION('',(0.,1.,0.)) ;
#3244 = DIRECTION('center_axis',(0.,1.,0.)) ;
#3245 = DIRECTION('ref_axis',(-0.479425538604204,0.,0.877582561890372)) ;
#3246 = DIRECTION('center_axis',(-0.877582561890372,0.,-0.479425538604204)) ;
#3247 = DIRECTION('ref_axis',(0.479425538604204,0.,-0.877582561890372)) ;
#3248 = DIRECTION('center_axis',(0.,-1.,0.)) ;
#3249 = DIRECTION('ref_axis',(-0.479425538604204,0.,0.877582561890372)) ;
#3250 = DIRECTION('center_axis',(0.,-1.,0.)) ;
#3251 = DIRECTION('ref_axis',(0.,0.,1.)) ;
#3252 = DIRECTION('',(0.,-1.,0.)) ;
#3253 = DIRECTION('center_axis',(0.,-1.,0.)) ;
#3254 = DIRECTION('ref_axis',(1.,0.,0.)) ;
#3255 = DIRECTION('center_axis',(0.,-1.,0.)) ;
#3256 = DIRECTION('ref_axis',(0.,0.,1.)) ;
#3257 = DIRECTION('center_axis',(0.,-1.,0.)) ;
#3258 = DIRECTION('ref_axis',(-0.479425538604204,0.,0.877582561890372)) ;
#3259 = DIRECTION('center_axis',(0.877582561890372,0.,0.479425538604204)) ;
#3260 = DIRECTION('ref_axis',(0.479425538604204,0.,-0.877582561890372)) ;
#3261 = DIRECTION('',(2.77555756156289E-17,-2.16840434497178E-19,1.)) ;
#3262 = DIRECTION('',(1.,5.55111512312578E-17,-2.77555756156289E-17)) ;
#3263 = DIRECTION('',(0.,0.,1.)) ;
#3264 = DIRECTION('',(1.,-4.27642353614751E-50,0.)) ;
#3265 = DIRECTION('',(0.,0.,1.)) ;
#3266 = DIRECTION('',(1.,-4.27642353614751E-50,0.)) ;
#3267 = DIRECTION('',(0.,0.,1.)) ;
#3268 = DIRECTION('',(1.,-4.27642353614751E-50,0.)) ;
#3269 = DIRECTION('',(0.176493191114639,0.429898151293963,0.885459052132963)) ;
#3270 = DIRECTION('',(0.409943370649535,-0.849952837581464,0.33094804236876)) ;
#3271 = DIRECTION('',(-0.929327739695482,0.0277990986766462,0.368208042206106)) ;
#3272 = DIRECTION('',(0.273707299755107,-0.617475307129508,0.737433765938398)) ;
#3273 = DIRECTION('',(-0.740217141731164,-0.0796010570858149,0.667639314898521)) ;
#3274 = DIRECTION('',(0.281748688195291,-0.938304495733796,0.200505236804377)) ;
#3275 = DIRECTION('',(-0.635912052105926,-0.763702588047179,0.111239466901236)) ;
#3276 = DIRECTION('',(0.362798339606772,-0.168597139444709,0.916489153972719)) ;
#3277 = DIRECTION('',(-0.609676698314986,-0.743592970776257,0.274524711718049)) ;
#3278 = DIRECTION('',(0.476265239907167,-0.0668046392025062,0.876760264517725)) ;
#3279 = DIRECTION('',(0.0720839514673508,-0.457419972652013,0.886324360806971)) ;
#3280 = DIRECTION('',(0.770284466384301,0.590051128823483,0.241870846157996)) ;
#3281 = DIRECTION('',(-0.431127569509108,0.206095232815885,-0.87843825839938)) ;
#3282 = DIRECTION('',(-0.676112180934338,-0.718483260175436,0.163260906649113)) ;
#3283 = CARTESIAN_POINT('',(0.,0.,0.)) ;
#3284 = CARTESIAN_POINT('',(0.,0.,0.)) ;
#3285 = CARTESIAN_POINT('Origin',(-434.543858273742,156.789736278414,-59.8178313623822)) ;
#3286 = CARTESIAN_POINT('',(-436.338218860625,162.960256993635,-58.8406189048122)) ;
#3287 = CARTESIAN_POINT('Origin',(-438.475999931612,159.134353154959,-60.2253036738863)) ;
#3288 = CARTESIAN_POINT('',(-429.816865801527,160.758779287006,-57.7801268294347)) ;
#3289 = CARTESIAN_POINT('Origin',(-434.543858273742,156.789736278414,-59.8178313623822)) ;
#3290 = CARTESIAN_POINT('Origin',(-432.661711545155,155.667469237209,-59.6227919297228)) ;
#3291 = CARTESIAN_POINT('Origin',(-439.841577868686,159.948605884407,-60.3668131226735)) ;
#3292 = CARTESIAN_POINT('',(-438.44621833762,162.445826698405,-59.4630100549641)) ;
#3293 = CARTESIAN_POINT('Origin',(-439.841577868686,159.948605884407,-60.3668131226735)) ;
#3294 = CARTESIAN_POINT('',(-438.44621833762,162.445826698405,-59.4630100549641)) ;
#3295 = CARTESIAN_POINT('Origin',(-440.660835141651,160.437104162332,-60.4517095185253)) ;
#3296 = CARTESIAN_POINT('',(-440.08473288355,163.422823254255,-59.6328028466676)) ;
#3297 = CARTESIAN_POINT('Origin',(-441.480092414616,160.925602440257,-60.536605914377)) ;
#3298 = CARTESIAN_POINT('',(-439.265475610585,162.93432497633,-59.5479064508159)) ;
#3299 = CARTESIAN_POINT('Origin',(-441.480092414616,160.925602440257,-60.536605914377)) ;
#3300 = CARTESIAN_POINT('',(-440.7078892807,165.565759008383,-59.2934305940894)) ;
#3301 = CARTESIAN_POINT('',(-440.08473288355,163.422823254255,-59.6328028466676)) ;
#3302 = CARTESIAN_POINT('Origin',(-442.84567035169,161.739855169706,-60.6781153631642)) ;
#3303 = CARTESIAN_POINT('Origin',(-446.77781200956,164.08447204625,-61.0855876746684)) ;
#3304 = CARTESIAN_POINT('',(-445.815112994521,170.298049137252,-59.4379620070397)) ;
#3305 = CARTESIAN_POINT('Origin',(-448.659958738148,165.206739087456,-61.2806271073278)) ;
#3306 = CARTESIAN_POINT('Origin',(-446.77781200956,164.08447204625,-61.0855876746684)) ;
#3307 = CARTESIAN_POINT('Origin',(-432.661711545155,155.667469237209,-59.6227919297228)) ;
#3308 = CARTESIAN_POINT('',(-436.391179339219,149.00477156037,-58.5866958081163)) ;
#3309 = CARTESIAN_POINT('Origin',(-432.405055173074,155.514432822499,-59.596195643451)) ;
#3310 = CARTESIAN_POINT('',(-436.741766535065,148.876355333483,-58.5690042756859)) ;
#3311 = CARTESIAN_POINT('Origin',(-436.6478357113,149.15780797508,-58.6132920943881)) ;
#3312 = CARTESIAN_POINT('',(-428.887033553867,162.285813775497,-57.209108680316)) ;
#3313 = CARTESIAN_POINT('Origin',(-432.604270565142,155.633218922022,-59.6168395478055)) ;
#3314 = CARTESIAN_POINT('Origin',(-432.604270565142,155.633218922022,-59.6168395478055)) ;
#3315 = CARTESIAN_POINT('Origin',(-448.659958738148,165.206739087456,-61.2806271073278)) ;
#3316 = CARTESIAN_POINT('',(-445.000162706884,171.893584256118,-58.8788486217556)) ;
#3317 = CARTESIAN_POINT('',(-452.603568779148,158.444505266078,-62.892048462345)) ;
#3318 = CARTESIAN_POINT('Origin',(-448.71739971816,165.240989402643,-61.2865794892451)) ;
#3319 = CARTESIAN_POINT('Origin',(-448.71739971816,165.240989402643,-61.2865794892451)) ;
#3320 = CARTESIAN_POINT('',(-452.660607254351,158.811943224256,-62.8539556969519)) ;
#3321 = CARTESIAN_POINT('Origin',(-452.403950882271,158.658906809546,-62.8273594106802)) ;
#3322 = CARTESIAN_POINT('Origin',(-448.916615110228,165.359775502165,-61.3072233935995)) ;
#3323 = CARTESIAN_POINT('Origin',(-434.174324018733,156.569394203754,-59.7795379868709)) ;
#3324 = CARTESIAN_POINT('',(-436.700167681604,164.284821180549,-58.625284827235)) ;
#3325 = CARTESIAN_POINT('Origin',(-434.174324018733,156.569394203754,-59.7795379868709)) ;
#3326 = CARTESIAN_POINT('',(-442.156244262532,155.147161163856,-58.5522636076438)) ;
#3327 = CARTESIAN_POINT('Origin',(-439.302650006998,159.627259536871,-60.3109661566578)) ;
#3328 = CARTESIAN_POINT('Origin',(-439.302650006998,159.627259536871,-60.3109661566578)) ;
#3329 = CARTESIAN_POINT('Origin',(-439.490271689493,159.739132658813,-60.3304086506742)) ;
#3330 = CARTESIAN_POINT('',(-442.29526604286,155.335335372473,-58.6016587733327)) ;
#3331 = CARTESIAN_POINT('Origin',(-442.448265734862,155.095128247764,-58.5073633254777)) ;
#3332 = CARTESIAN_POINT('',(-436.932112549205,164.317370817808,-58.6734363598735)) ;
#3333 = CARTESIAN_POINT('Origin',(-439.490271689493,159.739132658813,-60.3304086506742)) ;
#3334 = CARTESIAN_POINT('Origin',(-439.490271689493,159.739132658813,-60.3304086506742)) ;
#3335 = CARTESIAN_POINT('Origin',(-447.147346264569,164.304814120911,-61.1238810501796)) ;
#3336 = CARTESIAN_POINT('',(-444.872614531839,156.766850414779,-58.8337503313788)) ;
#3337 = CARTESIAN_POINT('',(-439.416537950911,165.904510431472,-58.9067715509699)) ;
#3338 = CARTESIAN_POINT('Origin',(-442.019020276305,161.246948787794,-60.5924528803928)) ;
#3339 = CARTESIAN_POINT('Origin',(-447.147346264569,164.304814120911,-61.1238810501796)) ;
#3340 = CARTESIAN_POINT('Origin',(-442.019020276305,161.246948787794,-60.5924528803928)) ;
#3341 = CARTESIAN_POINT('Origin',(-440.660835141651,160.437104162332,-60.4517095185253)) ;
#3342 = CARTESIAN_POINT('',(-439.273239453521,165.713313824847,-58.9160380955758)) ;
#3343 = CARTESIAN_POINT('',(-438.102676001363,165.015342321328,-58.7947372277247)) ;
#3344 = CARTESIAN_POINT('',(-444.636392947176,156.731278379512,-58.8442605090349)) ;
#3345 = CARTESIAN_POINT('Origin',(-441.831398593809,161.135075665852,-60.5730103863764)) ;
#3346 = CARTESIAN_POINT('Origin',(-441.831398593809,161.135075665852,-60.5730103863764)) ;
#3347 = CARTESIAN_POINT('Origin',(-441.831398593809,161.135075665852,-60.5730103863764)) ;
#3348 = CARTESIAN_POINT('Origin',(-444.789392639178,156.491071254803,-58.7499650611799)) ;
#3349 = CARTESIAN_POINT('Origin',(-440.660835141651,160.437104162332,-60.4517095185253)) ;
#3350 = CARTESIAN_POINT('',(-429.731313677501,160.707767148769,-57.7712614006774)) ;
#3351 = CARTESIAN_POINT('',(-437.815989398024,165.528414212129,-58.6090444182372)) ;
#3352 = CARTESIAN_POINT('Origin',(-432.576159421128,155.616457098972,-59.6139265009655)) ;
#3353 = CARTESIAN_POINT('Origin',(-436.509323339471,148.894285480052,-58.0823390440383)) ;
#3354 = CARTESIAN_POINT('',(-429.46718544632,160.77222427359,-57.6932770653741)) ;
#3355 = CARTESIAN_POINT('Origin',(-432.405055173074,155.514432822499,-59.596195643451)) ;
#3356 = CARTESIAN_POINT('Origin',(-432.576159421128,155.616457098972,-59.6139265009655)) ;
#3357 = CARTESIAN_POINT('Origin',(-429.638289708763,160.874248536369,-57.7110078628301)) ;
#3358 = CARTESIAN_POINT('Origin',(-440.660835141651,160.437104162332,-60.4517095185253)) ;
#3359 = CARTESIAN_POINT('',(-451.711778518624,160.062091415581,-62.5608600391744)) ;
#3360 = CARTESIAN_POINT('',(-445.900665118548,170.349061275489,-59.446827435797)) ;
#3361 = CARTESIAN_POINT('Origin',(-448.745510862175,165.257751225692,-61.289492536085)) ;
#3362 = CARTESIAN_POINT('Origin',(-448.745510862175,165.257751225692,-61.289492536085)) ;
#3363 = CARTESIAN_POINT('',(-437.815989398024,165.528414212129,-58.6090444182372)) ;
#3364 = CARTESIAN_POINT('Origin',(-453.020883276625,158.739628159719,-59.7933667941868)) ;
#3365 = CARTESIAN_POINT('',(-451.979877125812,159.994222158519,-62.6201635025592)) ;
#3366 = CARTESIAN_POINT('Origin',(-448.916615110228,165.359775502165,-61.3072233935995)) ;
#3367 = CARTESIAN_POINT('Origin',(-448.745510862175,165.257751225692,-61.289492536085)) ;
#3368 = CARTESIAN_POINT('Origin',(-451.808772877759,159.892197882045,-62.6024326450446)) ;
#3369 = CARTESIAN_POINT('',(0.,0.,0.)) ;
#3370 = CARTESIAN_POINT('Origin',(-415.730955726499,145.572172760385,-57.8683245658292)) ;
#3371 = CARTESIAN_POINT('',(-418.171335668733,142.669556598323,-54.8039516305242)) ;
#3372 = CARTESIAN_POINT('Origin',(-416.01793220457,145.743288135211,-57.8980628049471)) ;
#3373 = CARTESIAN_POINT('',(-417.627137271938,142.865595422292,-55.143801917793)) ;
#3374 = CARTESIAN_POINT('',(-417.627137271938,142.865595422292,-55.143801917793)) ;
#3375 = CARTESIAN_POINT('Origin',(-415.730955726499,145.572172760385,-57.8683245658292)) ;
#3376 = CARTESIAN_POINT('Origin',(-414.179234039917,148.075085772684,-58.4406760839186)) ;
#3377 = CARTESIAN_POINT('',(-417.059123981534,143.676367947338,-55.9599500750264)) ;
#3378 = CARTESIAN_POINT('Origin',(-415.730955726499,145.572172760385,-57.8683245658292)) ;
#3379 = CARTESIAN_POINT('Origin',(-426.211090919796,151.821159694385,-58.9543395885945)) ;
#3380 = CARTESIAN_POINT('',(-424.869313254862,146.663357598784,-55.4980365966556)) ;
#3381 = CARTESIAN_POINT('Origin',(-422.715909790697,149.73708913567,-58.5921477710773)) ;
#3382 = CARTESIAN_POINT('',(-428.36449438396,148.747428157499,-55.8602284141728)) ;
#3383 = CARTESIAN_POINT('Origin',(-426.211090919796,151.821159694385,-58.9543395885945)) ;
#3384 = CARTESIAN_POINT('',(-432.372954182314,152.807540691692,-57.5468618225734)) ;
#3385 = CARTESIAN_POINT('',(-427.539259174831,149.925354881338,-57.0459650977917)) ;
#3386 = CARTESIAN_POINT('Origin',(-431.044785927279,154.703345504738,-59.4552363133763)) ;
#3387 = CARTESIAN_POINT('Origin',(-423.002886268769,149.908204510497,-58.6218860101951)) ;
#3388 = CARTESIAN_POINT('',(-424.899067814208,147.201627172404,-55.8973633621589)) ;
#3389 = CARTESIAN_POINT('',(-424.899067814208,147.201627172404,-55.8973633621589)) ;
#3390 = CARTESIAN_POINT('Origin',(-423.002886268769,149.908204510497,-58.6218860101951)) ;
#3391 = CARTESIAN_POINT('Origin',(-431.044785927279,154.703345504738,-59.4552363133763)) ;
#3392 = CARTESIAN_POINT('',(-433.801022573454,152.673545780845,-56.9446442256091)) ;
#3393 = CARTESIAN_POINT('',(-432.372954182314,152.807540691691,-57.5468618225734)) ;
#3394 = CARTESIAN_POINT('Origin',(-431.985859291572,155.264479025341,-59.552756029706)) ;
#3395 = CARTESIAN_POINT('Origin',(-420.787544940893,153.481529987722,-59.4390131941874)) ;
#3396 = CARTESIAN_POINT('',(-425.15628973293,146.834472973614,-55.5277748357752)) ;
#3397 = CARTESIAN_POINT('Origin',(-423.002886268769,149.908204510497,-58.6218860101951)) ;
#3398 = CARTESIAN_POINT('Origin',(-426.211090919796,151.821159694385,-58.9543395885945)) ;
#3399 = CARTESIAN_POINT('',(-438.506389394923,155.479213383858,-57.4322428072573)) ;
#3400 = CARTESIAN_POINT('',(-428.026254201678,149.230226449888,-56.3462277844973)) ;
#3401 = CARTESIAN_POINT('Origin',(-436.691226113041,158.070146628355,-60.0403546113545)) ;
#3402 = CARTESIAN_POINT('Origin',(-426.211090919796,151.821159694385,-58.9543395885945)) ;
#3403 = CARTESIAN_POINT('',(-426.011810973197,147.344594355981,-55.6164291233476)) ;
#3404 = CARTESIAN_POINT('Origin',(-423.858407509036,150.418325892863,-58.7105402977676)) ;
#3405 = CARTESIAN_POINT('',(-428.36449438396,148.747428157499,-55.8602284141728)) ;
#3406 = CARTESIAN_POINT('Origin',(-421.342549414525,154.476382190137,-59.6385128924298)) ;
#3407 = CARTESIAN_POINT('',(-427.233563764187,145.637241385156,-53.650610998181)) ;
#3408 = CARTESIAN_POINT('',(-427.414274787281,144.019732278968,-61.2139661498883)) ;
#3409 = CARTESIAN_POINT('',(-427.323919275734,144.828486832062,-57.4322885740347)) ;
#3410 = CARTESIAN_POINT('',(-424.039118532129,148.800816786675,-66.2738954494749)) ;
#3411 = CARTESIAN_POINT('',(-425.726696659705,146.41027453282,-63.7439307996865)) ;
#3412 = CARTESIAN_POINT('',(-420.483251253884,155.19941040057,-63.7704695973542)) ;
#3413 = CARTESIAN_POINT('',(-422.261184893006,152.000113593621,-65.0221825234194)) ;
#3414 = CARTESIAN_POINT('',(-420.302540230791,156.816919506758,-56.2071144456468)) ;
#3415 = CARTESIAN_POINT('',(-420.392895742337,156.008164953664,-59.9887920215005)) ;
#3416 = CARTESIAN_POINT('',(-423.677696485943,152.035834999051,-51.1471851460603)) ;
#3417 = CARTESIAN_POINT('',(-421.990118358366,154.426377252906,-53.6771497958487)) ;
#3418 = CARTESIAN_POINT('',(-425.455630125065,148.836538192105,-52.3988980721158)) ;
#3419 = CARTESIAN_POINT('Origin',(-427.260853379936,158.160697256591,-60.2850395075904)) ;
#3420 = CARTESIAN_POINT('',(-426.29118891266,160.387769183321,-56.8276944586541)) ;
#3421 = CARTESIAN_POINT('',(-429.666345167812,155.606684675614,-51.7677651590675)) ;
#3422 = CARTESIAN_POINT('',(-427.978767040236,157.997226929469,-54.2977298088559)) ;
#3423 = CARTESIAN_POINT('',(-426.471899935753,158.770260077133,-64.3910496103614)) ;
#3424 = CARTESIAN_POINT('',(-426.381544424206,159.579014630227,-60.6093720345077)) ;
#3425 = CARTESIAN_POINT('',(-430.027767213998,152.371666463237,-66.8944754624821)) ;
#3426 = CARTESIAN_POINT('',(-428.249833574876,155.570963270184,-65.6427625364266)) ;
#3427 = CARTESIAN_POINT('',(-433.40292346915,147.590581955531,-61.8345461628956)) ;
#3428 = CARTESIAN_POINT('',(-431.715345341574,149.981124209383,-64.3645108126938)) ;
#3429 = CARTESIAN_POINT('',(-433.222212446057,149.208091061719,-54.2711910111883)) ;
#3430 = CARTESIAN_POINT('',(-433.312567957603,148.399336508625,-58.0528685870419)) ;
#3431 = CARTESIAN_POINT('',(-431.444278806934,152.407387868668,-53.019478085123)) ;
#3432 = CARTESIAN_POINT('',(-431.927853123794,151.01908136232,-56.341333608517)) ;
#3433 = CARTESIAN_POINT('Origin',(-429.847056190905,153.989175569426,-59.3311203107748)) ;
#3434 = CARTESIAN_POINT('Origin',(-420.483251253884,155.19941040057,-63.7704695973542)) ;
#3435 = CARTESIAN_POINT('',(-423.296864571725,158.602344345039,-56.5174044521504)) ;
#3436 = CARTESIAN_POINT('',(-423.477575594818,156.984835238851,-64.0807596038578)) ;
#3437 = CARTESIAN_POINT('',(-424.219383064324,158.512786394731,-59.4101157634537)) ;
#3438 = CARTESIAN_POINT('',(-422.50834058379,157.492543629999,-59.2328071883088)) ;
#3439 = CARTESIAN_POINT('Origin',(-423.363861824057,158.002665012365,-59.3214614758812)) ;
#3440 = CARTESIAN_POINT('',(-424.266099582754,158.094635953892,-61.3653568676994)) ;
#3441 = CARTESIAN_POINT('',(-424.242741323539,158.303711174311,-60.3877363155766)) ;
#3442 = CARTESIAN_POINT('',(-422.55505710222,157.074393189159,-61.1880482925545)) ;
#3443 = CARTESIAN_POINT('Origin',(-423.410578342487,157.584514571526,-61.276702580127)) ;
#3444 = CARTESIAN_POINT('',(-422.531698843005,157.283468409579,-60.2104277404316)) ;
#3445 = CARTESIAN_POINT('Origin',(-423.669198623584,157.167362402809,-61.1813106604454)) ;
#3446 = CARTESIAN_POINT('',(-423.072297664414,156.240088851726,-60.9972644531914)) ;
#3447 = CARTESIAN_POINT('',(-422.813677383317,156.657241020443,-61.092656372873)) ;
#3448 = CARTESIAN_POINT('',(-424.783340144948,157.260331616459,-61.1745730283363)) ;
#3449 = CARTESIAN_POINT('',(-424.524719863851,157.677483785175,-61.2699649480179)) ;
#3450 = CARTESIAN_POINT('Origin',(-423.927818904681,156.750210234093,-61.0859187407639)) ;
#3451 = CARTESIAN_POINT('Origin',(-422.55505710222,157.074393189159,-61.1880482925545)) ;
#3452 = CARTESIAN_POINT('',(-423.025581145983,156.658239292566,-59.0420233489456)) ;
#3453 = CARTESIAN_POINT('',(-422.766960864886,157.075391461282,-59.1374152686272)) ;
#3454 = CARTESIAN_POINT('',(-423.048939405199,156.449164072146,-60.0196439010685)) ;
#3455 = CARTESIAN_POINT('Origin',(-424.219383064324,158.512786394731,-59.4101157634537)) ;
#3456 = CARTESIAN_POINT('',(-424.736623626517,157.678482057298,-59.2193319240906)) ;
#3457 = CARTESIAN_POINT('',(-424.47800334542,158.095634226015,-59.3147238437721)) ;
#3458 = CARTESIAN_POINT('',(-424.759981885733,157.469406836878,-60.1969524762134)) ;
#3459 = CARTESIAN_POINT('Origin',(-420.910136304531,155.173860616231,-59.7980081821374)) ;
#3460 = CARTESIAN_POINT('Origin',(-423.88110238625,157.168360674932,-59.1306776365181)) ;
#3461 = CARTESIAN_POINT('Origin',(-423.622482105153,157.585512843649,-59.2260695561997)) ;
#3462 = CARTESIAN_POINT('Origin',(-424.039118532129,148.800816786675,-66.2738954494749)) ;
#3463 = CARTESIAN_POINT('',(-427.033442873063,150.586241624956,-66.5841854559785)) ;
#3464 = CARTESIAN_POINT('',(-426.570653070541,153.468593453358,-65.7447134420378)) ;
#3465 = CARTESIAN_POINT('',(-425.651407877875,155.122726175179,-65.0975401929532)) ;
#3466 = CARTESIAN_POINT('',(-426.111030474208,154.295659814269,-65.4211268174955)) ;
#3467 = CARTESIAN_POINT('',(-424.859610590007,152.448350688626,-65.5674048668929)) ;
#3468 = CARTESIAN_POINT('Origin',(-425.715131830274,152.958472070992,-65.6560591544653)) ;
#3469 = CARTESIAN_POINT('',(-423.940365397341,154.102483410447,-64.9202316178083)) ;
#3470 = CARTESIAN_POINT('',(-424.399987993674,153.275417049536,-65.2438182423506)) ;
#3471 = CARTESIAN_POINT('Origin',(-424.795886637608,154.612604792813,-65.0088859053807)) ;
#3472 = CARTESIAN_POINT('Origin',(-420.302540230791,156.816919506758,-56.2071144456468)) ;
#3473 = CARTESIAN_POINT('',(-426.672020826877,153.821259837333,-51.4574751525639)) ;
#3474 = CARTESIAN_POINT('',(-425.403699602451,157.339914614044,-54.7301280175053)) ;
#3475 = CARTESIAN_POINT('',(-426.276228276686,156.103932333062,-53.4220601623442)) ;
#3476 = CARTESIAN_POINT('',(-425.839963939568,156.721923473553,-54.0760940899247)) ;
#3477 = CARTESIAN_POINT('',(-423.692657121916,156.319671849312,-54.5528194423604)) ;
#3478 = CARTESIAN_POINT('Origin',(-424.548178362183,156.829793231678,-54.6414737299329)) ;
#3479 = CARTESIAN_POINT('',(-424.565185796152,155.08368956833,-53.2447515871992)) ;
#3480 = CARTESIAN_POINT('',(-424.128921459034,155.701680708821,-53.8987855147798)) ;
#3481 = CARTESIAN_POINT('Origin',(-425.420707036419,155.593810950696,-53.3334058747717)) ;
#3482 = CARTESIAN_POINT('Origin',(-427.414274787281,144.019732278968,-61.2139661498883)) ;
#3483 = CARTESIAN_POINT('',(-430.408599128215,145.805157117249,-61.524256156392)) ;
#3484 = CARTESIAN_POINT('',(-430.012806578024,148.087829612977,-63.488841166182)) ;
#3485 = CARTESIAN_POINT('',(-429.140277903789,149.323811893959,-64.7969090213432)) ;
#3486 = CARTESIAN_POINT('',(-429.576542240906,148.705820753468,-64.1428750937626)) ;
#3487 = CARTESIAN_POINT('',(-428.30176409749,147.067586848245,-63.3115325910371)) ;
#3488 = CARTESIAN_POINT('Origin',(-429.157285337757,147.577708230611,-63.4001868786096)) ;
#3489 = CARTESIAN_POINT('',(-427.429235423255,148.303569129226,-64.6196004461983)) ;
#3490 = CARTESIAN_POINT('',(-427.865499760372,147.685577988735,-63.9655665186177)) ;
#3491 = CARTESIAN_POINT('Origin',(-428.284756663522,148.813690511593,-64.7082547337707)) ;
#3492 = CARTESIAN_POINT('Origin',(-423.677696485943,152.035834999051,-51.1471851460603)) ;
#3493 = CARTESIAN_POINT('',(-430.227888105122,147.422666223438,-53.9609010046846)) ;
#3494 = CARTESIAN_POINT('',(-428.845853109934,151.959150773663,-52.4742557416495)) ;
#3495 = CARTESIAN_POINT('',(-429.765098302599,150.305018051842,-53.1214289907341)) ;
#3496 = CARTESIAN_POINT('',(-429.305475706267,151.132084412752,-52.7978423661918)) ;
#3497 = CARTESIAN_POINT('',(-427.1348106294,150.938908008931,-52.2969471665046)) ;
#3498 = CARTESIAN_POINT('Origin',(-427.990331869667,151.449029391297,-52.3856014540771)) ;
#3499 = CARTESIAN_POINT('',(-428.054055822065,149.284775287109,-52.9441204155892)) ;
#3500 = CARTESIAN_POINT('',(-427.594433225732,150.11184164802,-52.6205337910469)) ;
#3501 = CARTESIAN_POINT('Origin',(-428.909577062332,149.794896669476,-53.0327747031617)) ;
#3502 = CARTESIAN_POINT('Origin',(-427.233563764187,145.637241385156,-53.650610998181)) ;
#3503 = CARTESIAN_POINT('',(-431.15040659772,147.333108273129,-56.8536123159879)) ;
#3504 = CARTESIAN_POINT('',(-431.197123116151,146.91495783229,-58.8088534202336)) ;
#3505 = CARTESIAN_POINT('',(-431.173764856936,147.12403305271,-57.8312328681108)) ;
#3506 = CARTESIAN_POINT('',(-429.439364117186,146.312865508397,-56.676303740843)) ;
#3507 = CARTESIAN_POINT('Origin',(-430.294885357453,146.822986890763,-56.7649580284154)) ;
#3508 = CARTESIAN_POINT('',(-429.486080635617,145.894715067558,-58.6315448450887)) ;
#3509 = CARTESIAN_POINT('',(-429.462722376402,146.103790287977,-57.6539242929658)) ;
#3510 = CARTESIAN_POINT('Origin',(-430.341601875884,146.404836449924,-58.7201991326612)) ;
#3511 = CARTESIAN_POINT('Origin',(-430.036265076356,147.24013905948,-56.860349948097)) ;
#3512 = CARTESIAN_POINT('',(-428.922123554992,147.14716984583,-56.8670875802061)) ;
#3513 = CARTESIAN_POINT('',(-429.180743836089,146.730017677113,-56.7716956605245)) ;
#3514 = CARTESIAN_POINT('',(-430.633166035527,148.167412610562,-57.044396155351)) ;
#3515 = CARTESIAN_POINT('',(-430.891786316623,147.750260441846,-56.9490042356694)) ;
#3516 = CARTESIAN_POINT('Origin',(-429.77764479526,147.657291228196,-56.9557418677785)) ;
#3517 = CARTESIAN_POINT('Origin',(-422.55505710222,157.074393189159,-61.1880482925545)) ;
#3518 = CARTESIAN_POINT('',(-428.968840073423,146.729019404991,-58.8223286844518)) ;
#3519 = CARTESIAN_POINT('',(-429.22746035452,146.311867236274,-58.7269367647703)) ;
#3520 = CARTESIAN_POINT('',(-428.945481814208,146.93809462541,-57.844708132329)) ;
#3521 = CARTESIAN_POINT('Origin',(-424.219383064324,158.512786394731,-59.4101157634537)) ;
#3522 = CARTESIAN_POINT('',(-430.679882553957,147.749262169723,-58.9996372595968)) ;
#3523 = CARTESIAN_POINT('',(-430.938502835054,147.332110001006,-58.9042453399152)) ;
#3524 = CARTESIAN_POINT('',(-430.656524294742,147.958337390143,-58.0220167074739)) ;
#3525 = CARTESIAN_POINT('Origin',(-426.80667871354,145.662791169495,-57.6230724133978)) ;
#3526 = CARTESIAN_POINT('Origin',(-429.82436131369,147.239140787357,-58.9109829720243)) ;
#3527 = CARTESIAN_POINT('Origin',(-430.082981594787,146.82198861864,-58.8155910523427)) ;
#3528 = CARTESIAN_POINT('Origin',(-424.687602925666,156.530684921226,-55.0170998867998)) ;
#3529 = CARTESIAN_POINT('',(-423.971506248882,155.721455228409,-55.3040717560845)) ;
#3530 = CARTESIAN_POINT('',(-423.832081685399,156.020563538859,-54.9284455992273)) ;
#3531 = CARTESIAN_POINT('',(-425.682548729416,156.741697993141,-55.4813803312294)) ;
#3532 = CARTESIAN_POINT('',(-425.543124165933,157.040806303592,-55.1057541743722)) ;
#3533 = CARTESIAN_POINT('Origin',(-424.827027489149,156.231576610775,-55.3927260436569)) ;
#3534 = CARTESIAN_POINT('Origin',(-422.55505710222,157.074393189159,-61.1880482925545)) ;
#3535 = CARTESIAN_POINT('',(-424.844034923117,154.485472947427,-53.9960039009233)) ;
#3536 = CARTESIAN_POINT('',(-424.704610359635,154.784581257878,-53.6203777440662)) ;
#3537 = CARTESIAN_POINT('',(-424.407770586,155.103464087918,-54.6500378285039)) ;
#3538 = CARTESIAN_POINT('Origin',(-424.219383064324,158.512786394731,-59.4101157634537)) ;
#3539 = CARTESIAN_POINT('',(-426.555077403651,155.505715712159,-54.1733124760682)) ;
#3540 = CARTESIAN_POINT('',(-426.415652840169,155.80482402261,-53.7976863192111)) ;
#3541 = CARTESIAN_POINT('',(-426.118813066534,156.12370685265,-54.8273464036488)) ;
#3542 = CARTESIAN_POINT('Origin',(-422.268967485332,153.828160632003,-54.4284021095727)) ;
#3543 = CARTESIAN_POINT('Origin',(-425.699556163384,154.995594329793,-54.0846581884958)) ;
#3544 = CARTESIAN_POINT('Origin',(-425.560131599902,155.294702640244,-53.7090320316386)) ;
#3545 = CARTESIAN_POINT('Origin',(-429.017860774274,147.876816541063,-63.0245607217426)) ;
#3546 = CARTESIAN_POINT('',(-428.022914970524,147.665803469147,-62.560280277313)) ;
#3547 = CARTESIAN_POINT('',(-428.162339534007,147.366695158697,-62.9359064341702)) ;
#3548 = CARTESIAN_POINT('',(-429.733957451058,148.68604623388,-62.737588852458)) ;
#3549 = CARTESIAN_POINT('',(-429.873382014541,148.386937923429,-63.1132150093151)) ;
#3550 = CARTESIAN_POINT('Origin',(-428.878436210791,148.175924851514,-62.6489345648855)) ;
#3551 = CARTESIAN_POINT('Origin',(-422.55505710222,157.074393189159,-61.1880482925545)) ;
#3552 = CARTESIAN_POINT('',(-427.150386296289,148.901785750129,-63.8683481324742)) ;
#3553 = CARTESIAN_POINT('',(-427.289810859772,148.602677439679,-64.2439742893313)) ;
#3554 = CARTESIAN_POINT('',(-427.586650633407,148.283794609638,-63.2143142048936)) ;
#3555 = CARTESIAN_POINT('Origin',(-424.219383064324,158.512786394731,-59.4101157634537)) ;
#3556 = CARTESIAN_POINT('',(-428.861428776823,149.922028514862,-64.0456567076191)) ;
#3557 = CARTESIAN_POINT('',(-429.000853340306,149.622920204411,-64.4212828644763)) ;
#3558 = CARTESIAN_POINT('',(-429.297693113941,149.304037374371,-63.3916227800385)) ;
#3559 = CARTESIAN_POINT('Origin',(-425.447847532739,147.008491153723,-62.9926784859625)) ;
#3560 = CARTESIAN_POINT('Origin',(-428.005907536556,149.411907132495,-63.9570024200467)) ;
#3561 = CARTESIAN_POINT('Origin',(-428.145332100039,149.112798822045,-64.3326285769038)) ;
#3562 = CARTESIAN_POINT('Origin',(-425.834327547888,152.840428212728,-65.1850410779168)) ;
#3563 = CARTESIAN_POINT('',(-425.098002025235,152.212262972096,-64.6253687138057)) ;
#3564 = CARTESIAN_POINT('',(-424.978806307621,152.330306830362,-65.0963867903444)) ;
#3565 = CARTESIAN_POINT('',(-426.809044505769,153.232505736828,-64.8026772889506)) ;
#3566 = CARTESIAN_POINT('',(-426.689848788155,153.350549595094,-65.2736953654893)) ;
#3567 = CARTESIAN_POINT('Origin',(-425.953523265502,152.722384354462,-64.7140230013782)) ;
#3568 = CARTESIAN_POINT('Origin',(-422.55505710222,157.074393189159,-61.1880482925545)) ;
#3569 = CARTESIAN_POINT('',(-424.178756832569,153.866395693917,-63.9781954647211)) ;
#3570 = CARTESIAN_POINT('',(-424.059561114955,153.984439552183,-64.4492135412598)) ;
#3571 = CARTESIAN_POINT('',(-424.638379428902,153.039329333006,-64.3017820892634)) ;
#3572 = CARTESIAN_POINT('Origin',(-424.219383064324,158.512786394731,-59.4101157634537)) ;
#3573 = CARTESIAN_POINT('',(-425.889799313103,154.886638458649,-64.155504039866)) ;
#3574 = CARTESIAN_POINT('',(-425.770603595489,155.004682316915,-64.6265221164047)) ;
#3575 = CARTESIAN_POINT('',(-426.349421909436,154.059572097739,-64.4790906644083)) ;
#3576 = CARTESIAN_POINT('Origin',(-422.499576328234,151.764025877091,-64.0801463703322)) ;
#3577 = CARTESIAN_POINT('Origin',(-425.034278072836,154.376517076283,-64.0668497522936)) ;
#3578 = CARTESIAN_POINT('Origin',(-424.915082355222,154.494560934549,-64.5378678288323)) ;
#3579 = CARTESIAN_POINT('Origin',(-427.871136152053,151.567073249561,-52.8566195306256)) ;
#3580 = CARTESIAN_POINT('',(-426.896419194171,151.174995725461,-53.2389833195918)) ;
#3581 = CARTESIAN_POINT('',(-427.015614911786,151.056951867195,-52.7679652430531)) ;
#3582 = CARTESIAN_POINT('',(-428.607461674705,152.195238490193,-53.4162918947367)) ;
#3583 = CARTESIAN_POINT('',(-428.72665739232,152.077194631927,-52.945273818198)) ;
#3584 = CARTESIAN_POINT('Origin',(-427.751940434438,151.685117107827,-53.3276376071643)) ;
#3585 = CARTESIAN_POINT('Origin',(-422.55505710222,157.074393189159,-61.1880482925545)) ;
#3586 = CARTESIAN_POINT('',(-427.815664386837,149.520863003639,-53.8861565686764)) ;
#3587 = CARTESIAN_POINT('',(-427.934860104451,149.402819145373,-53.4151384921377)) ;
#3588 = CARTESIAN_POINT('',(-427.356041790504,150.34792936455,-53.5625699441341)) ;
#3589 = CARTESIAN_POINT('Origin',(-424.219383064324,158.512786394731,-59.4101157634537)) ;
#3590 = CARTESIAN_POINT('',(-429.526706867371,150.541105768372,-54.0634651438213)) ;
#3591 = CARTESIAN_POINT('',(-429.645902584985,150.423061910106,-53.5924470672826)) ;
#3592 = CARTESIAN_POINT('',(-429.067084271038,151.368172129282,-53.739878519279)) ;
#3593 = CARTESIAN_POINT('Origin',(-425.217238689837,149.072625908635,-53.3409342252029)) ;
#3594 = CARTESIAN_POINT('Origin',(-428.671185627104,150.030984386006,-53.9748108562489)) ;
#3595 = CARTESIAN_POINT('Origin',(-428.790381344718,149.91294052774,-53.5037927797102)) ;
#3596 = CARTESIAN_POINT('Origin',(-434.570539808047,161.49079441183,-60.8225683527433)) ;
#3597 = CARTESIAN_POINT('',(-433.741264095171,162.693309250613,-61.9058149407666)) ;
#3598 = CARTESIAN_POINT('Origin',(-436.691226113041,158.070146628355,-60.0403546113545)) ;
#3599 = CARTESIAN_POINT('Origin',(-436.434569740961,157.917110213645,-60.0137583250828)) ;
#3600 = CARTESIAN_POINT('',(-433.433353664221,162.818524604835,-61.9789632008915)) ;
#3601 = CARTESIAN_POINT('Origin',(-433.484607723091,162.540272835903,-61.8792186544949)) ;
#3602 = CARTESIAN_POINT('',(-439.214726609873,154.133897479889,-56.1600302115885)) ;
#3603 = CARTESIAN_POINT('Origin',(-436.52605577973,157.97166056537,-60.0232386619911)) ;
#3604 = CARTESIAN_POINT('Origin',(-436.52605577973,157.97166056537,-60.0232386619911)) ;
#3605 = CARTESIAN_POINT('Origin',(-426.211090919796,151.821159694385,-58.9543395885945)) ;
#3606 = CARTESIAN_POINT('',(-428.175935754834,158.45348503928,-59.7105799665025)) ;
#3607 = CARTESIAN_POINT('',(-432.681825203754,151.468652058629,-56.4194647576367)) ;
#3608 = CARTESIAN_POINT('Origin',(-430.601028270865,154.438746265736,-59.4092514598946)) ;
#3609 = CARTESIAN_POINT('',(-428.291887852685,148.851065487279,-55.9645528863367)) ;
#3610 = CARTESIAN_POINT('Origin',(-430.601028270865,154.438746265736,-59.4092514598946)) ;
#3611 = CARTESIAN_POINT('Origin',(-434.543858272972,156.789736277955,-59.8178313623023)) ;
#3612 = CARTESIAN_POINT('',(-432.890930981183,151.522189137641,-56.3869745462188)) ;
#3613 = CARTESIAN_POINT('Origin',(-434.543858272972,156.789736277955,-59.8178313623023)) ;
#3614 = CARTESIAN_POINT('',(-428.308909482746,158.625038695568,-59.7336968330844)) ;
#3615 = CARTESIAN_POINT('Origin',(-430.774976653306,154.542466413331,-59.4272770438238)) ;
#3616 = CARTESIAN_POINT('Origin',(-430.774976653306,154.542466413331,-59.4272770438238)) ;
#3617 = CARTESIAN_POINT('Origin',(-430.601028270865,154.438746265736,-59.4092514598946)) ;
#3618 = CARTESIAN_POINT('Origin',(-428.021142615512,158.709744960995,-59.7298137009669)) ;
#3619 = CARTESIAN_POINT('',(0.,0.,0.)) ;
#3620 = CARTESIAN_POINT('Origin',(-408.672905494227,141.363671355823,-57.1369266933493)) ;
#3621 = CARTESIAN_POINT('',(-408.181726471869,148.672541235612,-55.3525040279398)) ;
#3622 = CARTESIAN_POINT('Origin',(-411.367797401137,142.970553710317,-57.4161876992097)) ;
#3623 = CARTESIAN_POINT('',(-420.672336579767,156.120313418157,-56.6468566264977)) ;
#3624 = CARTESIAN_POINT('',(-405.486834564959,147.065658881117,-55.0732430220794)) ;
#3625 = CARTESIAN_POINT('Origin',(-423.858407509036,150.418325892863,-58.7105402977676)) ;
#3626 = CARTESIAN_POINT('Origin',(-408.672905494227,141.363671355823,-57.1369266933493)) ;
#3627 = CARTESIAN_POINT('',(-405.668306122096,146.230582638267,-55.3071569860444)) ;
#3628 = CARTESIAN_POINT('Origin',(-408.459025184229,141.236141010272,-57.1147631214633)) ;
#3629 = CARTESIAN_POINT('',(-408.577078339004,147.964995338312,-55.6085815637908)) ;
#3630 = CARTESIAN_POINT('',(-405.882186432094,146.358112983818,-55.3293205579304)) ;
#3631 = CARTESIAN_POINT('Origin',(-411.367797401137,142.970553710317,-57.4161876992097)) ;
#3632 = CARTESIAN_POINT('Origin',(-403.75365836276,138.430473407259,-56.6271645398148)) ;
#3633 = CARTESIAN_POINT('',(-402.590858753538,140.511490752257,-55.8739953167236)) ;
#3634 = CARTESIAN_POINT('',(-402.590858753538,140.511490752257,-55.8739953167236)) ;
#3635 = CARTESIAN_POINT('Origin',(-403.75365836276,138.430473407259,-56.6271645398148)) ;
#3636 = CARTESIAN_POINT('Origin',(-408.672905494227,141.363671355823,-57.1369266933493)) ;
#3637 = CARTESIAN_POINT('',(-392.581260242414,134.543070578573,-54.8367401521258)) ;
#3638 = CARTESIAN_POINT('Origin',(-393.744059851636,132.462053233575,-55.589909375217)) ;
#3639 = CARTESIAN_POINT('',(-407.510105885005,143.444688700821,-56.3837574702581)) ;
#3640 = CARTESIAN_POINT('Origin',(-393.487403479556,132.309016818865,-55.5633130889452)) ;
#3641 = CARTESIAN_POINT('',(-392.464139823441,134.140312082463,-54.900524172625)) ;
#3642 = CARTESIAN_POINT('',(-392.464139823441,134.140312082463,-54.9005241726249)) ;
#3643 = CARTESIAN_POINT('Origin',(-393.487403479556,132.309016818865,-55.5633130889452)) ;
#3644 = CARTESIAN_POINT('Origin',(-393.744059851636,132.462053233575,-55.589909375217)) ;
#3645 = CARTESIAN_POINT('',(-393.278940007947,133.294460171574,-55.2886416859805)) ;
#3646 = CARTESIAN_POINT('Origin',(-393.744059851636,132.462053233575,-55.589909375217)) ;
#3647 = CARTESIAN_POINT('',(-392.882747682761,133.391145838264,-55.1716650929378)) ;
#3648 = CARTESIAN_POINT('',(-393.278940007947,133.294460171574,-55.2886416859805)) ;
#3649 = CARTESIAN_POINT('Origin',(-393.487403479556,132.309016818865,-55.5633130889452)) ;
#3650 = CARTESIAN_POINT('Origin',(-408.672905494227,141.363671355823,-57.1369266933493)) ;
#3651 = CARTESIAN_POINT('',(-404.999580999606,140.28312310999,-56.5032054257232)) ;
#3652 = CARTESIAN_POINT('Origin',(-405.464700843295,139.450716171991,-56.8044731149597)) ;
#3653 = CARTESIAN_POINT('',(-408.207785650538,142.196078293822,-56.8356590041128)) ;
#3654 = CARTESIAN_POINT('Origin',(-405.464700843295,139.450716171991,-56.8044731149597)) ;
#3655 = CARTESIAN_POINT('',(-407.458827108158,145.35616437361,-55.9355726289835)) ;
#3656 = CARTESIAN_POINT('',(-404.999580999606,140.28312310999,-56.5032054257232)) ;
#3657 = CARTESIAN_POINT('Origin',(-409.435586443835,141.818434887114,-57.2159603082382)) ;
#3658 = CARTESIAN_POINT('Origin',(-408.672905494227,141.363671355823,-57.1369266933493)) ;
#3659 = CARTESIAN_POINT('',(-408.193308329086,145.794113261501,-56.0116840173532)) ;
#3660 = CARTESIAN_POINT('Origin',(-410.170067664763,142.256383775005,-57.2920716966082)) ;
#3661 = CARTESIAN_POINT('',(-406.69614615855,144.90140084232,-55.8565390140943)) ;
#3662 = CARTESIAN_POINT('Origin',(-410.457044142834,142.427499149831,-57.3218099357261)) ;
#3663 = CARTESIAN_POINT('',(-408.464935852315,145.992698065281,-56.0314804227262)) ;
#3664 = CARTESIAN_POINT('Origin',(-410.457044142834,142.427499149831,-57.3218099357261)) ;
#3665 = CARTESIAN_POINT('',(-407.907724745062,146.305211121435,-55.8267056561618)) ;
#3666 = CARTESIAN_POINT('',(-408.464935852315,145.992698065282,-56.0314804227263)) ;
#3667 = CARTESIAN_POINT('Origin',(-410.170067664763,142.256383775005,-57.2920716966082)) ;
#3668 = CARTESIAN_POINT('Origin',(-408.672905494227,141.363671355823,-57.1369266933493)) ;
#3669 = CARTESIAN_POINT('',(-419.801105043013,152.752112123184,-57.2062028680609)) ;
#3670 = CARTESIAN_POINT('Origin',(-421.793213333533,149.186913207734,-58.4965323810607)) ;
#3671 = CARTESIAN_POINT('',(-406.680797203708,144.928870271273,-55.8465971803495)) ;
#3672 = CARTESIAN_POINT('Origin',(-421.793213333533,149.186913207734,-58.4965323810607)) ;
#3673 = CARTESIAN_POINT('',(-419.821765810054,153.560117818126,-57.0268932764394)) ;
#3674 = CARTESIAN_POINT('',(-419.801105043014,152.752112123185,-57.2062028680609)) ;
#3675 = CARTESIAN_POINT('Origin',(-422.147365028502,149.39808312813,-58.5332317226227)) ;
#3676 = CARTESIAN_POINT('Origin',(-408.672905494227,141.363671355823,-57.1369266933493)) ;
#3677 = CARTESIAN_POINT('',(-421.361704042538,154.478336306385,-57.1864709940707)) ;
#3678 = CARTESIAN_POINT('Origin',(-423.687303260982,150.31630161639,-58.6928094402531)) ;
#3679 = CARTESIAN_POINT('',(-406.347306275783,145.525706045819,-55.6305882471669)) ;
#3680 = CARTESIAN_POINT('Origin',(-423.687303260982,150.31630161639,-58.6928094402531)) ;
#3681 = CARTESIAN_POINT('',(-421.439784321854,154.746841970458,-57.1439483137379)) ;
#3682 = CARTESIAN_POINT('',(-421.361704042538,154.478336306386,-57.1864709940707)) ;
#3683 = CARTESIAN_POINT('Origin',(-423.858407509036,150.418325892863,-58.7105402977676)) ;
#3684 = CARTESIAN_POINT('Origin',(-414.910895252164,137.255568998901,-56.1093183995723)) ;
#3685 = CARTESIAN_POINT('Origin',(-394.625332716382,130.473547276512,-55.1435886423464)) ;
#3686 = CARTESIAN_POINT('Origin',(-412.368340054087,138.710590340914,-56.481240379315)) ;
#3687 = CARTESIAN_POINT('Origin',(-426.548058432443,146.079943338211,-57.7184643330794)) ;
#3688 = CARTESIAN_POINT('Origin',(-419.401620616319,145.13262479315,-57.6866191692542)) ;
#3689 = CARTESIAN_POINT('',(-419.418928880099,145.248588743018,-57.9803074161011)) ;
#3690 = CARTESIAN_POINT('Origin',(-419.487172740346,145.183636931387,-57.6954845980114)) ;
#3691 = CARTESIAN_POINT('',(-412.553607560257,141.155005746794,-57.2688812797066)) ;
#3692 = CARTESIAN_POINT('',(-419.333376756073,145.197576604781,-57.9714419873439)) ;
#3693 = CARTESIAN_POINT('Ctrl Pts',(-412.676919232686,141.2339336726,-56.7092671151722)) ;
#3694 = CARTESIAN_POINT('Ctrl Pts',(-412.726221526063,141.220486185843,-56.7000347274095)) ;
#3695 = CARTESIAN_POINT('Ctrl Pts',(-412.780237048048,141.203418744776,-56.6975093825531)) ;
#3696 = CARTESIAN_POINT('Ctrl Pts',(-412.883694241173,141.165398454256,-56.7113289821998)) ;
#3697 = CARTESIAN_POINT('Ctrl Pts',(-412.933141915367,141.144467080632,-56.7276880576375)) ;
#3698 = CARTESIAN_POINT('Ctrl Pts',(-413.009081951286,141.107464069561,-56.7731191552882)) ;
#3699 = CARTESIAN_POINT('Ctrl Pts',(-413.041997367993,141.089077365977,-56.8026459175359)) ;
#3700 = CARTESIAN_POINT('Ctrl Pts',(-413.076606466844,141.064863662361,-56.8567831525088)) ;
#3701 = CARTESIAN_POINT('Ctrl Pts',(-413.085785778931,141.057328086883,-56.8764350833939)) ;
#3702 = CARTESIAN_POINT('Ctrl Pts',(-413.098405249366,141.044070922671,-56.9175614950294)) ;
#3703 = CARTESIAN_POINT('Ctrl Pts',(-413.101846592404,141.038349309035,-56.9390356042263)) ;
#3704 = CARTESIAN_POINT('Ctrl Pts',(-413.102874041078,141.029152816437,-56.9820377359598)) ;
#3705 = CARTESIAN_POINT('Ctrl Pts',(-413.100473082469,141.025562152055,-57.0041071627164)) ;
#3706 = CARTESIAN_POINT('Ctrl Pts',(-413.089875154383,141.020724885159,-57.0475889973176)) ;
#3707 = CARTESIAN_POINT('Ctrl Pts',(-413.081676984783,141.019478445686,-57.0690011307828)) ;
#3708 = CARTESIAN_POINT('Ctrl Pts',(-413.04981465685,141.019106338779,-57.1298253609199)) ;
#3709 = CARTESIAN_POINT('Ctrl Pts',(-413.018463263424,141.02349377516,-57.1657581557835)) ;
#3710 = CARTESIAN_POINT('Ctrl Pts',(-412.945042397752,141.037948184903,-57.2257626809506)) ;
#3711 = CARTESIAN_POINT('Ctrl Pts',(-412.896600259782,141.049879199996,-57.251488628588)) ;
#3712 = CARTESIAN_POINT('Ctrl Pts',(-412.794258470493,141.077915728419,-57.2843523756985)) ;
#3713 = CARTESIAN_POINT('Ctrl Pts',(-412.740353258286,141.09399580819,-57.2914945502996)) ;
#3714 = CARTESIAN_POINT('Ctrl Pts',(-412.645590273407,141.123769060528,-57.2902200682869)) ;
#3715 = CARTESIAN_POINT('Ctrl Pts',(-412.596828621117,141.139796832197,-57.2830215450146)) ;
#3716 = CARTESIAN_POINT('Ctrl Pts',(-412.505050414036,141.172088889752,-57.2530168351479)) ;
#3717 = CARTESIAN_POINT('Ctrl Pts',(-412.462009546431,141.188351512697,-57.2302832756091)) ;
#3718 = CARTESIAN_POINT('Ctrl Pts',(-412.402535340985,141.213954732135,-57.1811079957144)) ;
#3719 = CARTESIAN_POINT('Ctrl Pts',(-412.378983312568,141.225294776528,-57.1548298739571)) ;
#3720 = CARTESIAN_POINT('Ctrl Pts',(-412.345902244053,141.245901273597,-57.094749541473)) ;
#3721 = CARTESIAN_POINT('Ctrl Pts',(-412.336529826198,141.255181308432,-57.0608658812438)) ;
#3722 = CARTESIAN_POINT('Ctrl Pts',(-412.334946143032,141.269356547435,-56.9945834927675)) ;
#3723 = CARTESIAN_POINT('Ctrl Pts',(-412.342670191364,141.274830746562,-56.9594774261293)) ;
#3724 = CARTESIAN_POINT('Ctrl Pts',(-412.372769961544,141.280909269161,-56.8947805439396)) ;
#3725 = CARTESIAN_POINT('Ctrl Pts',(-412.394985379514,141.281532964064,-56.8651170892932)) ;
#3726 = CARTESIAN_POINT('Ctrl Pts',(-412.451898726647,141.278851487698,-56.8071119626716)) ;
#3727 = CARTESIAN_POINT('Ctrl Pts',(-412.493695520927,141.273724322324,-56.7777769310266)) ;
#3728 = CARTESIAN_POINT('Ctrl Pts',(-412.583687827021,141.257417516029,-56.7330357665052)) ;
#3729 = CARTESIAN_POINT('Ctrl Pts',(-412.631910958312,141.246209940744,-56.7176954014261)) ;
#3730 = CARTESIAN_POINT('Ctrl Pts',(-412.676919232686,141.2339336726,-56.7092671151722)) ;
#3731 = CARTESIAN_POINT('Origin',(-414.148241431988,144.628448202997,-57.7043141338184)) ;
#3732 = CARTESIAN_POINT('',(-417.692863650504,148.184665926882,-57.7426394325392)) ;
#3733 = CARTESIAN_POINT('Origin',(-418.2975194473,147.102536907483,-58.1342874285466)) ;
#3734 = CARTESIAN_POINT('',(-420.259427371306,149.71503007398,-58.0086022952566)) ;
#3735 = CARTESIAN_POINT('',(-413.543585635193,145.710577222396,-57.312666137811)) ;
#3736 = CARTESIAN_POINT('Origin',(-420.864083168101,148.632901054581,-58.400250291264)) ;
#3737 = CARTESIAN_POINT('Origin',(-421.536495898953,147.548305415918,-58.1522313000919)) ;
#3738 = CARTESIAN_POINT('',(-420.538499277519,149.215585911181,-58.1893629087985)) ;
#3739 = CARTESIAN_POINT('Origin',(-420.864083168101,148.632901054581,-58.400250291264)) ;
#3740 = CARTESIAN_POINT('Origin',(-420.521874671994,148.428852501635,-58.364788576235)) ;
#3741 = CARTESIAN_POINT('',(-420.382338718888,148.678574583035,-58.2744082694641)) ;
#3742 = CARTESIAN_POINT('Origin',(-420.521874671994,148.428852501635,-58.364788576235)) ;
#3743 = CARTESIAN_POINT('',(-420.382338718887,148.678574583035,-58.2744082694641)) ;
#3744 = CARTESIAN_POINT('Origin',(-414.148241431988,144.628448202997,-57.7043141338184)) ;
#3745 = CARTESIAN_POINT('',(-407.292863742802,140.873717432833,-56.9179976696054)) ;
#3746 = CARTESIAN_POINT('',(-414.008705478881,144.878170284397,-57.6139338270475)) ;
#3747 = CARTESIAN_POINT('Origin',(-407.432399695909,140.623995351433,-57.0083779763764)) ;
#3748 = CARTESIAN_POINT('Origin',(-407.872054173773,139.914836664615,-56.8462117129177)) ;
#3749 = CARTESIAN_POINT('',(-407.037047828773,141.331541248732,-56.752300440525)) ;
#3750 = CARTESIAN_POINT('Origin',(-407.432399695909,140.623995351433,-57.0083779763764)) ;
#3751 = CARTESIAN_POINT('Origin',(-414.148241431988,144.628448202997,-57.7043141338184)) ;
#3752 = CARTESIAN_POINT('',(-410.031372169708,143.116966087014,-57.0625904470286)) ;
#3753 = CARTESIAN_POINT('',(-413.752889564853,145.335994100296,-57.4482365979674)) ;
#3754 = CARTESIAN_POINT('Origin',(-410.426724036843,142.409420189714,-57.31866798288)) ;
#3755 = CARTESIAN_POINT('Origin',(-414.148241431988,144.628448202997,-57.7043141338184)) ;
#3756 = CARTESIAN_POINT('',(-410.828799568389,146.58875613729,-56.4619379762644)) ;
#3757 = CARTESIAN_POINT('Origin',(-412.479975013484,143.633711507393,-57.5314382730539)) ;
#3758 = CARTESIAN_POINT('',(-412.197633552816,147.404950349076,-56.6037848363803)) ;
#3759 = CARTESIAN_POINT('',(-412.497065986893,147.583492832894,-56.6348138370289)) ;
#3760 = CARTESIAN_POINT('Origin',(-413.848808997911,144.449905719179,-57.6732851331698)) ;
#3761 = CARTESIAN_POINT('Origin',(-416.047081387235,140.904112285089,-56.8624538158766)) ;
#3762 = CARTESIAN_POINT('',(-411.872049662236,147.987635205673,-56.3928974539119)) ;
#3763 = CARTESIAN_POINT('Origin',(-413.848808997911,144.449905719179,-57.6732851331698)) ;
#3764 = CARTESIAN_POINT('Origin',(-414.148241431988,144.628448202997,-57.7043141338184)) ;
#3765 = CARTESIAN_POINT('',(-413.754196390824,149.109902246878,-56.5879368865713)) ;
#3766 = CARTESIAN_POINT('',(-412.171482096311,148.166177689494,-56.4239264545634)) ;
#3767 = CARTESIAN_POINT('Origin',(-415.730955726499,145.572172760384,-57.8683245658292)) ;
#3768 = CARTESIAN_POINT('Origin',(-417.28267741308,143.069259748086,-57.2959730477399)) ;
#3769 = CARTESIAN_POINT('',(-414.335596195432,148.069393574382,-56.9645214981198)) ;
#3770 = CARTESIAN_POINT('Origin',(-415.730955726499,145.572172760384,-57.8683245658292)) ;
#3771 = CARTESIAN_POINT('Origin',(-414.148241431988,144.628448202997,-57.7043141338184)) ;
#3772 = CARTESIAN_POINT('',(-416.902159916234,149.59975772148,-57.2304843608372)) ;
#3773 = CARTESIAN_POINT('',(-412.752881900922,147.125669016995,-56.800511066109)) ;
#3774 = CARTESIAN_POINT('Origin',(-418.2975194473,147.102536907483,-58.1342874285466)) ;
#3775 = CARTESIAN_POINT('Origin',(-419.849241133881,144.599623895184,-57.5619359104573)) ;
#3776 = CARTESIAN_POINT('',(-417.662499396266,147.829328416068,-60.0802875299202)) ;
#3777 = CARTESIAN_POINT('Origin',(-417.749219146275,147.645538655506,-60.3009705806305)) ;
#3778 = CARTESIAN_POINT('',(-417.811130065534,148.229693563362,-56.3422673396185)) ;
#3779 = CARTESIAN_POINT('Origin',(-417.656166455279,148.478435135556,-56.4064071069979)) ;
#3780 = CARTESIAN_POINT('Origin',(-410.426724036843,142.409420189714,-57.31866798288)) ;
#3781 = CARTESIAN_POINT('',(-410.031372169707,143.116966087013,-57.062590447029)) ;
#3782 = CARTESIAN_POINT('',(-411.18794426283,143.497751214042,-59.8327482012076)) ;
#3783 = CARTESIAN_POINT('',(-410.797178076421,143.735745419843,-59.3688613935254)) ;
#3784 = CARTESIAN_POINT('Ctrl Pts',(-411.187944262825,143.497751214042,-59.8327482012091)) ;
#3785 = CARTESIAN_POINT('Ctrl Pts',(-411.192211586621,143.519120254733,-59.8488679240781)) ;
#3786 = CARTESIAN_POINT('Ctrl Pts',(-411.194834914286,143.541552441395,-59.8632297300923)) ;
#3787 = CARTESIAN_POINT('Ctrl Pts',(-411.197337245685,143.603213566409,-59.8959336495249)) ;
#3788 = CARTESIAN_POINT('Ctrl Pts',(-411.193883331881,143.64812965929,-59.9121798889122)) ;
#3789 = CARTESIAN_POINT('Ctrl Pts',(-411.179107650862,143.714566933321,-59.9212739114798)) ;
#3790 = CARTESIAN_POINT('Ctrl Pts',(-411.172638140343,143.736590905115,-59.9218511079237)) ;
#3791 = CARTESIAN_POINT('Ctrl Pts',(-411.156996770963,143.778597502592,-59.917706412113)) ;
#3792 = CARTESIAN_POINT('Ctrl Pts',(-411.147825724058,143.798580515091,-59.9129853761654)) ;
#3793 = CARTESIAN_POINT('Ctrl Pts',(-411.127608522821,143.834960290994,-59.898751924725)) ;
#3794 = CARTESIAN_POINT('Ctrl Pts',(-411.116307830456,143.851815082021,-59.8890603076353)) ;
#3795 = CARTESIAN_POINT('Ctrl Pts',(-411.092171126716,143.881387006667,-59.8652001740172)) ;
#3796 = CARTESIAN_POINT('Ctrl Pts',(-411.079334607066,143.894103207011,-59.8510310149819)) ;
#3797 = CARTESIAN_POINT('Ctrl Pts',(-411.040061826278,143.924923258829,-59.8038854269408)) ;
#3798 = CARTESIAN_POINT('Ctrl Pts',(-411.012740311386,143.935385909337,-59.7659724610472)) ;
#3799 = CARTESIAN_POINT('Ctrl Pts',(-410.959733804494,143.939902382881,-59.6861601298485)) ;
#3800 = CARTESIAN_POINT('Ctrl Pts',(-410.931059528474,143.931407156765,-59.638658221865)) ;
#3801 = CARTESIAN_POINT('Ctrl Pts',(-410.879598412631,143.89577229749,-59.5468877200924)) ;
#3802 = CARTESIAN_POINT('Ctrl Pts',(-410.856788210741,143.868635778449,-59.5026310194625)) ;
#3803 = CARTESIAN_POINT('Ctrl Pts',(-410.822644525485,143.810126455096,-59.4312342708784)) ;
#3804 = CARTESIAN_POINT('Ctrl Pts',(-410.807844544746,143.775206429643,-59.3975338994376)) ;
#3805 = CARTESIAN_POINT('Ctrl Pts',(-410.797178076421,143.735745419843,-59.3688613935255)) ;
#3806 = CARTESIAN_POINT('Ctrl Pts',(-410.797178076421,143.735745419843,-59.3688613935255)) ;
#3807 = CARTESIAN_POINT('Ctrl Pts',(-410.796967543334,143.73496654459,-59.3682954600788)) ;
#3808 = CARTESIAN_POINT('Ctrl Pts',(-410.796758323441,143.734186086876,-59.3677313390647)) ;
#3809 = CARTESIAN_POINT('Ctrl Pts',(-410.785845388505,143.692982926168,-59.3381327400731)) ;
#3810 = CARTESIAN_POINT('Ctrl Pts',(-410.779463747391,143.647942683771,-59.3143744754051)) ;
#3811 = CARTESIAN_POINT('Ctrl Pts',(-410.778761937223,143.570997592292,-59.2881090138335)) ;
#3812 = CARTESIAN_POINT('Ctrl Pts',(-410.781594428872,143.534892229704,-59.2802214213014)) ;
#3813 = CARTESIAN_POINT('Ctrl Pts',(-410.796594740226,143.464927094214,-59.277305663745)) ;
#3814 = CARTESIAN_POINT('Ctrl Pts',(-410.808892850738,143.431090464959,-59.2823951324787)) ;
#3815 = CARTESIAN_POINT('Ctrl Pts',(-410.840055128798,143.375015606763,-59.3043342113034)) ;
#3816 = CARTESIAN_POINT('Ctrl Pts',(-410.860192135688,143.350486971278,-59.3220799344001)) ;
#3817 = CARTESIAN_POINT('Ctrl Pts',(-410.903855103505,143.314890663075,-59.3662962125199)) ;
#3818 = CARTESIAN_POINT('Ctrl Pts',(-410.927323217479,143.303669487857,-59.3927001361998)) ;
#3819 = CARTESIAN_POINT('Ctrl Pts',(-410.978415270172,143.289940024074,-59.4544416788403)) ;
#3820 = CARTESIAN_POINT('Ctrl Pts',(-411.009276655513,143.29093027168,-59.4954343394395)) ;
#3821 = CARTESIAN_POINT('Ctrl Pts',(-411.065829426459,143.308536877846,-59.5782479277446)) ;
#3822 = CARTESIAN_POINT('Ctrl Pts',(-411.091495321212,143.32522544883,-59.6200708925011)) ;
#3823 = CARTESIAN_POINT('Ctrl Pts',(-411.1121902565,143.345763576877,-59.6574526056856)) ;
#3824 = CARTESIAN_POINT('Ctrl Pts',(-411.134859594198,143.368261147123,-59.6984007250256)) ;
#3825 = CARTESIAN_POINT('Ctrl Pts',(-411.155499220532,143.399303501171,-59.7411292822976)) ;
#3826 = CARTESIAN_POINT('Ctrl Pts',(-411.177665344724,143.455729666604,-59.7984489428495)) ;
#3827 = CARTESIAN_POINT('Ctrl Pts',(-411.183640679057,143.476200597996,-59.816491507082)) ;
#3828 = CARTESIAN_POINT('Ctrl Pts',(-411.187944262825,143.497751214042,-59.8327482012091)) ;
#3829 = CARTESIAN_POINT('',(-410.853208211569,144.763179026854,-55.7816414442377)) ;
#3830 = CARTESIAN_POINT('',(-410.945808745689,144.136110567136,-55.6308412032236)) ;
#3831 = CARTESIAN_POINT('Ctrl Pts',(-410.853208211571,144.76317902685,-55.7816414442362)) ;
#3832 = CARTESIAN_POINT('Ctrl Pts',(-410.866101565596,144.776338152558,-55.7617595366245)) ;
#3833 = CARTESIAN_POINT('Ctrl Pts',(-410.879366221035,144.7870090043,-55.7411069784896)) ;
#3834 = CARTESIAN_POINT('Ctrl Pts',(-410.915234441741,144.808141922543,-55.6850287041196)) ;
#3835 = CARTESIAN_POINT('Ctrl Pts',(-410.940692427302,144.814359359455,-55.6449467921902)) ;
#3836 = CARTESIAN_POINT('Ctrl Pts',(-410.977468137829,144.805890096303,-55.5875817150653)) ;
#3837 = CARTESIAN_POINT('Ctrl Pts',(-410.989519327473,144.8002032316,-55.5688822109625)) ;
#3838 = CARTESIAN_POINT('Ctrl Pts',(-411.012251139134,144.783206221826,-55.5339429555556)) ;
#3839 = CARTESIAN_POINT('Ctrl Pts',(-411.022932248642,144.771897196056,-55.5177029769192)) ;
#3840 = CARTESIAN_POINT('Ctrl Pts',(-411.042122001205,144.744713912751,-55.488934296626)) ;
#3841 = CARTESIAN_POINT('Ctrl Pts',(-411.050872246538,144.728497413012,-55.4760433923461)) ;
#3842 = CARTESIAN_POINT('Ctrl Pts',(-411.065896965649,144.692010331772,-55.454379230945)) ;
#3843 = CARTESIAN_POINT('Ctrl Pts',(-411.072170663687,144.671739039288,-55.4456066332889)) ;
#3844 = CARTESIAN_POINT('Ctrl Pts',(-411.086696644048,144.607536787114,-55.4260618107772)) ;
#3845 = CARTESIAN_POINT('Ctrl Pts',(-411.090450063903,144.559939874016,-55.4223508921012)) ;
#3846 = CARTESIAN_POINT('Ctrl Pts',(-411.088241395851,144.464267219023,-55.4288286532431)) ;
#3847 = CARTESIAN_POINT('Ctrl Pts',(-411.080465387264,144.410212651786,-55.4418075470878)) ;
#3848 = CARTESIAN_POINT('Ctrl Pts',(-411.053736123842,144.310165122957,-55.4820064660659)) ;
#3849 = CARTESIAN_POINT('Ctrl Pts',(-411.034767278028,144.264167938495,-55.5092056101087)) ;
#3850 = CARTESIAN_POINT('Ctrl Pts',(-410.994978355097,144.193112909149,-55.5644745189731)) ;
#3851 = CARTESIAN_POINT('Ctrl Pts',(-410.971643135395,144.161135348259,-55.5962088184575)) ;
#3852 = CARTESIAN_POINT('Ctrl Pts',(-410.945808745689,144.136110567136,-55.6308412032236)) ;
#3853 = CARTESIAN_POINT('Ctrl Pts',(-410.945808745689,144.136110567136,-55.6308412032236)) ;
#3854 = CARTESIAN_POINT('Ctrl Pts',(-410.945298830537,144.135616631912,-55.6315247718287)) ;
#3855 = CARTESIAN_POINT('Ctrl Pts',(-410.944787948593,144.135125094846,-55.6322092502269)) ;
#3856 = CARTESIAN_POINT('Ctrl Pts',(-410.917835749852,144.109399975703,-55.6683294231447)) ;
#3857 = CARTESIAN_POINT('Ctrl Pts',(-410.888870545926,144.091437378252,-55.7066982382528)) ;
#3858 = CARTESIAN_POINT('Ctrl Pts',(-410.840788144812,144.078228038009,-55.7709205875192)) ;
#3859 = CARTESIAN_POINT('Ctrl Pts',(-410.818661134192,144.077445258792,-55.8006462833089)) ;
#3860 = CARTESIAN_POINT('Ctrl Pts',(-410.777412893653,144.09142781431,-55.8574943436152)) ;
#3861 = CARTESIAN_POINT('Ctrl Pts',(-410.758347903741,144.106361035004,-55.8846160834723)) ;
#3862 = CARTESIAN_POINT('Ctrl Pts',(-410.728769308847,144.148260654197,-55.928959393124)) ;
#3863 = CARTESIAN_POINT('Ctrl Pts',(-410.71704755088,144.176938464282,-55.947992188304)) ;
#3864 = CARTESIAN_POINT('Ctrl Pts',(-410.702613810583,144.241832332789,-55.9746208221084)) ;
#3865 = CARTESIAN_POINT('Ctrl Pts',(-410.699776826027,144.277977910514,-55.9823203715745)) ;
#3866 = CARTESIAN_POINT('Ctrl Pts',(-410.700029842929,144.358940062948,-55.9898023477557)) ;
#3867 = CARTESIAN_POINT('Ctrl Pts',(-410.705759375952,144.409817197619,-55.9862677279003)) ;
#3868 = CARTESIAN_POINT('Ctrl Pts',(-410.725284786663,144.507540195539,-55.96540453293)) ;
#3869 = CARTESIAN_POINT('Ctrl Pts',(-410.739117572465,144.554365057154,-55.9480121981902)) ;
#3870 = CARTESIAN_POINT('Ctrl Pts',(-410.754250710349,144.59430346092,-55.9274355227232)) ;
#3871 = CARTESIAN_POINT('Ctrl Pts',(-410.770827626794,144.638052192166,-55.9048957274367)) ;
#3872 = CARTESIAN_POINT('Ctrl Pts',(-410.791856738387,144.681130902918,-55.874607897007)) ;
#3873 = CARTESIAN_POINT('Ctrl Pts',(-410.827578363869,144.734108413478,-55.8209595835089)) ;
#3874 = CARTESIAN_POINT('Ctrl Pts',(-410.840205301136,144.749908086438,-55.8016922908536)) ;
#3875 = CARTESIAN_POINT('Ctrl Pts',(-410.853208211571,144.76317902685,-55.7816414442362)) ;
#3876 = CARTESIAN_POINT('Origin',(-417.663667022248,147.594526517269,-60.2921051518733)) ;
#3877 = CARTESIAN_POINT('',(-417.57694727224,147.778316277832,-60.071422101163)) ;
#3878 = CARTESIAN_POINT('Origin',(-417.570614331253,148.427422997319,-56.3975416782406)) ;
#3879 = CARTESIAN_POINT('',(-417.725577941508,148.178681425125,-56.3334019108612)) ;
#3880 = CARTESIAN_POINT('Origin',(-440.720031578363,158.18696279177,-59.9690769391319)) ;
#3881 = CARTESIAN_POINT('',(-438.755310766598,161.520385342634,-59.7481092393854)) ;
#3882 = CARTESIAN_POINT('Origin',(-439.685550453976,159.855571466636,-60.3506446178581)) ;
#3883 = CARTESIAN_POINT('',(-439.104150649365,160.896080139135,-59.9740600063125)) ;
#3884 = CARTESIAN_POINT('Origin',(-439.685550453976,159.855571466636,-60.3506446178581)) ;
#3885 = CARTESIAN_POINT('Origin',(-418.969932178152,146.01794126882,-57.8862684373746)) ;
#3886 = CARTESIAN_POINT('',(-417.344023767738,148.808971130381,-57.5166886656118)) ;
#3887 = CARTESIAN_POINT('Origin',(-418.2975194473,147.102536907483,-58.1342874285466)) ;
#3888 = CARTESIAN_POINT('',(-417.692863650503,148.184665926884,-57.7426394325401)) ;
#3889 = CARTESIAN_POINT('Origin',(-418.2975194473,147.102536907483,-58.1342874285466)) ;
#3890 = CARTESIAN_POINT('Origin',(-428.991534950723,153.479054187111,-59.2424660232112)) ;
#3891 = CARTESIAN_POINT('',(-420.601689255662,149.919110484244,-58.0440696072164)) ;
#3892 = CARTESIAN_POINT('',(-421.811000864351,147.754852430924,-58.8273655362774)) ;
#3893 = CARTESIAN_POINT('Origin',(-421.206345067555,148.836981450325,-58.4357175402709)) ;
#3894 = CARTESIAN_POINT('Origin',(-421.206345067555,148.836981450325,-58.4357175402709)) ;
#3895 = CARTESIAN_POINT('',(-428.386879153928,154.56118320651,-58.8508180272038)) ;
#3896 = CARTESIAN_POINT('Ctrl Pts',(-421.81100086462,147.754852431096,-58.8273655363048)) ;
#3897 = CARTESIAN_POINT('Ctrl Pts',(-421.853741332606,147.78033727655,-58.8317945622187)) ;
#3898 = CARTESIAN_POINT('Ctrl Pts',(-421.896094847306,147.806514641693,-58.835972949529)) ;
#3899 = CARTESIAN_POINT('Ctrl Pts',(-421.938043624344,147.833373922076,-58.8398988553431)) ;
#3900 = CARTESIAN_POINT('Ctrl Pts',(-421.979570384227,147.860903662599,-58.8435707517313)) ;
#3901 = CARTESIAN_POINT('Ctrl Pts',(-421.87615581497,147.692840521943,-58.5554346035487)) ;
#3902 = CARTESIAN_POINT('Ctrl Pts',(-421.918896282955,147.718325367397,-58.5598636294598)) ;
#3903 = CARTESIAN_POINT('Ctrl Pts',(-421.961208101147,147.744542417631,-58.5642160414727)) ;
#3904 = CARTESIAN_POINT('Ctrl Pts',(-422.003073485147,147.771481068213,-58.5684899967742)) ;
#3905 = CARTESIAN_POINT('Ctrl Pts',(-422.044475207505,147.799129814517,-58.5726837502117)) ;
#3906 = CARTESIAN_POINT('Ctrl Pts',(-421.904621272866,147.696490374139,-58.2597391318533)) ;
#3907 = CARTESIAN_POINT('Ctrl Pts',(-421.947361740345,147.721975220103,-58.2641681597162)) ;
#3908 = CARTESIAN_POINT('Ctrl Pts',(-421.989655341618,147.748189934754,-58.2687098055672)) ;
#3909 = CARTESIAN_POINT('Ctrl Pts',(-422.031484292327,147.775123913657,-58.2733622262356)) ;
#3910 = CARTESIAN_POINT('Ctrl Pts',(-422.072831387722,147.80276565509,-58.2781234408005)) ;
#3911 = CARTESIAN_POINT('Ctrl Pts',(-421.889780460918,147.772082270099,-57.9679944974231)) ;
#3912 = CARTESIAN_POINT('Ctrl Pts',(-421.932520929689,147.797567114102,-57.9724235241036)) ;
#3913 = CARTESIAN_POINT('Ctrl Pts',(-421.974824028932,147.823733452332,-57.9771518742023)) ;
#3914 = CARTESIAN_POINT('Ctrl Pts',(-422.016671974219,147.850570680443,-57.9821777047032)) ;
#3915 = CARTESIAN_POINT('Ctrl Pts',(-422.058047549007,147.878067356988,-57.9874988015613)) ;
#3916 = CARTESIAN_POINT('Ctrl Pts',(-421.727691708573,148.170743063868,-57.2382494781475)) ;
#3917 = CARTESIAN_POINT('Ctrl Pts',(-421.770432175108,148.196227912031,-57.2426785025898)) ;
#3918 = CARTESIAN_POINT('Ctrl Pts',(-421.812839003795,148.22213912497,-57.2478738591303)) ;
#3919 = CARTESIAN_POINT('Ctrl Pts',(-421.854894410256,148.248466098313,-57.2538337045393)) ;
#3920 = CARTESIAN_POINT('Ctrl Pts',(-421.896581048473,148.275197708994,-57.260555242246)) ;
#3921 = CARTESIAN_POINT('Ctrl Pts',(-421.300806933651,148.934613382335,-56.962373473136)) ;
#3922 = CARTESIAN_POINT('Ctrl Pts',(-421.343547404315,148.960098222817,-56.9668025016983)) ;
#3923 = CARTESIAN_POINT('Ctrl Pts',(-421.386227423225,148.985520587404,-56.9721744087365)) ;
#3924 = CARTESIAN_POINT('Ctrl Pts',(-421.428829206111,149.010869871353,-56.9784873518901)) ;
#3925 = CARTESIAN_POINT('Ctrl Pts',(-421.471335065955,149.036135561939,-56.9857383134319)) ;
#3926 = CARTESIAN_POINT('Ctrl Pts',(-420.968923911373,149.464677297305,-57.115056870481)) ;
#3927 = CARTESIAN_POINT('Ctrl Pts',(-421.011664377378,149.490162145958,-57.1194858972196)) ;
#3928 = CARTESIAN_POINT('Ctrl Pts',(-421.054556786388,149.515245293827,-57.1247600927859)) ;
#3929 = CARTESIAN_POINT('Ctrl Pts',(-421.09758335406,149.539916136489,-57.130877613928)) ;
#3930 = CARTESIAN_POINT('Ctrl Pts',(-421.140726128437,149.564164584178,-57.1378355657362)) ;
#3931 = CARTESIAN_POINT('Ctrl Pts',(-420.722334300366,149.804285292852,-57.5405450296813)) ;
#3932 = CARTESIAN_POINT('Ctrl Pts',(-420.765074768969,149.829770137461,-57.5449740545007)) ;
#3933 = CARTESIAN_POINT('Ctrl Pts',(-420.808124986228,149.854635948606,-57.5499759541758)) ;
#3934 = CARTESIAN_POINT('Ctrl Pts',(-420.851467167597,149.878872122105,-57.5555488858895)) ;
#3935 = CARTESIAN_POINT('Ctrl Pts',(-420.895083164411,149.90246883914,-57.5616902940697)) ;
#3936 = CARTESIAN_POINT('Ctrl Pts',(-420.601689255787,149.919110484538,-58.0440696068916)) ;
#3937 = CARTESIAN_POINT('Ctrl Pts',(-420.644429724086,149.944595329692,-58.0484986315046)) ;
#3938 = CARTESIAN_POINT('Ctrl Pts',(-420.687557149156,149.969387657571,-58.0531782959234)) ;
#3939 = CARTESIAN_POINT('Ctrl Pts',(-420.73105374647,149.993476863986,-58.0581067571802)) ;
#3940 = CARTESIAN_POINT('Ctrl Pts',(-420.774901271003,150.016853221822,-58.0632818619355)) ;
#3941 = CARTESIAN_POINT('',(-421.979570384495,147.860903662772,-58.8435707517587)) ;
#3942 = CARTESIAN_POINT('',(-420.774901269911,150.016853221085,-58.0632818618408)) ;
#3943 = CARTESIAN_POINT('Ctrl Pts',(-421.979570384227,147.860903662599,-58.8435707517313)) ;
#3944 = CARTESIAN_POINT('Ctrl Pts',(-421.991728913092,147.849331654895,-58.7928258723717)) ;
#3945 = CARTESIAN_POINT('Ctrl Pts',(-422.002346252811,147.84051778158,-58.7410831476083)) ;
#3946 = CARTESIAN_POINT('Ctrl Pts',(-422.011341475327,147.834528590436,-58.6887406204753)) ;
#3947 = CARTESIAN_POINT('Ctrl Pts',(-422.020433103031,147.828475210875,-58.6358371187712)) ;
#3948 = CARTESIAN_POINT('Ctrl Pts',(-422.027867607628,147.825307398783,-58.5823212873917)) ;
#3949 = CARTESIAN_POINT('Ctrl Pts',(-422.033587759229,147.825048295654,-58.5286122421676)) ;
#3950 = CARTESIAN_POINT('Ctrl Pts',(-422.039326113949,147.824788367987,-58.4747322797561)) ;
#3951 = CARTESIAN_POINT('Ctrl Pts',(-422.043339169569,147.827455647482,-58.4206582947106)) ;
#3952 = CARTESIAN_POINT('Ctrl Pts',(-422.045595964448,147.833028188724,-58.366815344478)) ;
#3953 = CARTESIAN_POINT('Ctrl Pts',(-422.047853400612,147.838602313442,-58.3129570943925)) ;
#3954 = CARTESIAN_POINT('Ctrl Pts',(-422.048353573025,147.847083285091,-58.2593304370043)) ;
#3955 = CARTESIAN_POINT('Ctrl Pts',(-422.047092431553,147.858404736773,-58.2063563350565)) ;
#3956 = CARTESIAN_POINT('Ctrl Pts',(-422.045834620582,147.869696290064,-58.1535221304005)) ;
#3957 = CARTESIAN_POINT('Ctrl Pts',(-422.042824794565,147.883813253942,-58.1013374569823)) ;
#3958 = CARTESIAN_POINT('Ctrl Pts',(-422.038085680684,147.900646799821,-58.0502092009584)) ;
#3959 = CARTESIAN_POINT('Ctrl Pts',(-422.033390570825,147.917324041432,-57.9995556853568)) ;
#3960 = CARTESIAN_POINT('Ctrl Pts',(-422.026998175001,147.93666752218,-57.9499394416247)) ;
#3961 = CARTESIAN_POINT('Ctrl Pts',(-422.018956495247,147.958530842599,-57.9017396362965)) ;
#3962 = CARTESIAN_POINT('Ctrl Pts',(-422.010998890888,147.980165583,-57.8540437577363)) ;
#3963 = CARTESIAN_POINT('Ctrl Pts',(-422.001426349376,148.004267619985,-57.8077352039805)) ;
#3964 = CARTESIAN_POINT('Ctrl Pts',(-421.990310280786,148.030657100577,-57.7631597452683)) ;
#3965 = CARTESIAN_POINT('Ctrl Pts',(-421.979286679813,148.056827063597,-57.718955081897)) ;
#3966 = CARTESIAN_POINT('Ctrl Pts',(-421.966745154894,148.085246463539,-57.6764551336579)) ;
#3967 = CARTESIAN_POINT('Ctrl Pts',(-421.952779447948,148.11570407895,-57.6359706624812)) ;
#3968 = CARTESIAN_POINT('Ctrl Pts',(-421.940433622346,148.142628917739,-57.6001819822066)) ;
#3969 = CARTESIAN_POINT('Ctrl Pts',(-421.926975175981,148.171146034768,-57.565968132908)) ;
#3970 = CARTESIAN_POINT('Ctrl Pts',(-421.912484514256,148.201086851866,-57.5335232033393)) ;
#3971 = CARTESIAN_POINT('Ctrl Pts',(-421.896469974511,148.234176328008,-57.4976662753414)) ;
#3972 = CARTESIAN_POINT('Ctrl Pts',(-421.879196136062,148.269000982753,-57.4639750106296)) ;
#3973 = CARTESIAN_POINT('Ctrl Pts',(-421.860784881679,148.305312756406,-57.4327011158411)) ;
#3974 = CARTESIAN_POINT('Ctrl Pts',(-421.842112703721,148.34213913909,-57.4009840086437)) ;
#3975 = CARTESIAN_POINT('Ctrl Pts',(-421.822270770487,148.380494869169,-57.3717533115999)) ;
#3976 = CARTESIAN_POINT('Ctrl Pts',(-421.801403243559,148.42010078959,-57.3452246979226)) ;
#3977 = CARTESIAN_POINT('Ctrl Pts',(-421.780249681462,148.460249595912,-57.3183324514799)) ;
#3978 = CARTESIAN_POINT('Ctrl Pts',(-421.75804236051,148.501682853816,-57.2942169071462)) ;
#3979 = CARTESIAN_POINT('Ctrl Pts',(-421.734946751139,148.544092520253,-57.2730543408166)) ;
#3980 = CARTESIAN_POINT('Ctrl Pts',(-421.711554780111,148.587046385321,-57.2516202175384)) ;
#3981 = CARTESIAN_POINT('Ctrl Pts',(-421.687251738192,148.631001603399,-57.2332153732183)) ;
#3982 = CARTESIAN_POINT('Ctrl Pts',(-421.662222814826,148.675624522545,-57.2179731713502)) ;
#3983 = CARTESIAN_POINT('Ctrl Pts',(-421.636685277877,148.721154225512,-57.2024212321921)) ;
#3984 = CARTESIAN_POINT('Ctrl Pts',(-421.610392226587,148.767378743309,-57.1901618736898)) ;
#3985 = CARTESIAN_POINT('Ctrl Pts',(-421.583551601739,148.813933965481,-57.1812842046049)) ;
#3986 = CARTESIAN_POINT('Ctrl Pts',(-421.556710976892,148.860489187653,-57.17240653552)) ;
#3987 = CARTESIAN_POINT('Ctrl Pts',(-421.529322989585,148.90737477357,-57.16691047875)) ;
#3988 = CARTESIAN_POINT('Ctrl Pts',(-421.501603772458,148.95422189431,-57.1648332412647)) ;
#3989 = CARTESIAN_POINT('Ctrl Pts',(-421.473633497548,149.001493317592,-57.1627371898772)) ;
#3990 = CARTESIAN_POINT('Ctrl Pts',(-421.445326175544,149.048725223269,-57.1641221705782)) ;
#3991 = CARTESIAN_POINT('Ctrl Pts',(-421.416909044811,149.095539089243,-57.1689740118675)) ;
#3992 = CARTESIAN_POINT('Ctrl Pts',(-421.38842807649,149.142458120102,-57.1738367525629)) ;
#3993 = CARTESIAN_POINT('Ctrl Pts',(-421.359837027396,149.188956868258,-57.1821818934184)) ;
#3994 = CARTESIAN_POINT('Ctrl Pts',(-421.331366585001,149.234660067844,-57.1939432467292)) ;
#3995 = CARTESIAN_POINT('Ctrl Pts',(-421.302964536217,149.28025347613,-57.205676346126)) ;
#3996 = CARTESIAN_POINT('Ctrl Pts',(-421.274682736938,149.32505479751,-57.2208091745726)) ;
#3997 = CARTESIAN_POINT('Ctrl Pts',(-421.246748794467,149.368702620244,-57.2392255460869)) ;
#3998 = CARTESIAN_POINT('Ctrl Pts',(-421.218938200403,149.412157706508,-57.257560596101)) ;
#3999 = CARTESIAN_POINT('Ctrl Pts',(-421.191472613444,149.454469114634,-57.2791501540304)) ;
#4000 = CARTESIAN_POINT('Ctrl Pts',(-421.16457196597,149.495296490057,-57.3038309247386)) ;
#4001 = CARTESIAN_POINT('Ctrl Pts',(-421.137930807612,149.535730036312,-57.3282736197127)) ;
#4002 = CARTESIAN_POINT('Ctrl Pts',(-421.111843941636,149.574707731227,-57.3557480443583)) ;
#4003 = CARTESIAN_POINT('Ctrl Pts',(-421.086517329051,149.611919830462,-57.3860495768582)) ;
#4004 = CARTESIAN_POINT('Ctrl Pts',(-421.079319379369,149.622495694762,-57.3946614236062)) ;
#4005 = CARTESIAN_POINT('Ctrl Pts',(-421.072182779199,149.632929093572,-57.403501342566)) ;
#4006 = CARTESIAN_POINT('Ctrl Pts',(-421.065112107606,149.643213281796,-57.4125639715692)) ;
#4007 = CARTESIAN_POINT('Ctrl Pts',(-421.040325659206,149.679264807793,-57.4443332855853)) ;
#4008 = CARTESIAN_POINT('Ctrl Pts',(-421.01636439484,149.7134588299,-57.478823639632)) ;
#4009 = CARTESIAN_POINT('Ctrl Pts',(-420.993412426575,149.74553265389,-57.5157706937358)) ;
#4010 = CARTESIAN_POINT('Ctrl Pts',(-420.970680376631,149.777299156895,-57.5523637331431)) ;
#4011 = CARTESIAN_POINT('Ctrl Pts',(-420.948938522522,149.806985666695,-57.591366512365)) ;
#4012 = CARTESIAN_POINT('Ctrl Pts',(-420.928351251074,149.834367925265,-57.6324838549583)) ;
#4013 = CARTESIAN_POINT('Ctrl Pts',(-420.907763979626,149.861750183835,-57.6736011975515)) ;
#4014 = CARTESIAN_POINT('Ctrl Pts',(-420.888331463762,149.886827906802,-57.716833071087)) ;
#4015 = CARTESIAN_POINT('Ctrl Pts',(-420.870201102755,149.909411860059,-57.7618467009588)) ;
#4016 = CARTESIAN_POINT('Ctrl Pts',(-420.852668002297,149.931251840027,-57.8053774665191)) ;
#4017 = CARTESIAN_POINT('Ctrl Pts',(-420.836352736448,149.950759582813,-57.8505743243232)) ;
#4018 = CARTESIAN_POINT('Ctrl Pts',(-420.821371186243,149.967798922127,-57.8971032240582)) ;
#4019 = CARTESIAN_POINT('Ctrl Pts',(-420.806644593601,149.98454828421,-57.9428402901869)) ;
#4020 = CARTESIAN_POINT('Ctrl Pts',(-420.79320680203,149.998912402389,-57.989864350575)) ;
#4021 = CARTESIAN_POINT('Ctrl Pts',(-420.781149569571,150.010797939994,-58.0378276646215)) ;
#4022 = CARTESIAN_POINT('Ctrl Pts',(-420.779023792142,150.012893446376,-58.0462839443498)) ;
#4023 = CARTESIAN_POINT('Ctrl Pts',(-420.776940879598,150.014912002863,-58.0547693444178)) ;
#4024 = CARTESIAN_POINT('Ctrl Pts',(-420.774901271003,150.016853221822,-58.0632818619345)) ;
#4025 = CARTESIAN_POINT('Origin',(-422.462167734146,146.589483527618,-59.2491443977063)) ;
#4026 = CARTESIAN_POINT('Origin',(-419.950521499685,151.084480165857,-57.6222947862863)) ;
#4027 = CARTESIAN_POINT('Ctrl Pts',(-420.601751328529,149.919051417961,-58.0438104715933)) ;
#4028 = CARTESIAN_POINT('Ctrl Pts',(-420.644495899909,149.944538709794,-58.0482399216921)) ;
#4029 = CARTESIAN_POINT('Ctrl Pts',(-420.687627462681,149.969333389136,-58.0529202253984)) ;
#4030 = CARTESIAN_POINT('Ctrl Pts',(-420.731128227209,149.993424848719,-58.0578495392067)) ;
#4031 = CARTESIAN_POINT('Ctrl Pts',(-420.774979943197,150.016803358696,-58.0630257089282)) ;
#4032 = CARTESIAN_POINT('Ctrl Pts',(-420.49059208657,150.024888462511,-58.5075145316237)) ;
#4033 = CARTESIAN_POINT('Ctrl Pts',(-420.533336657653,150.050375754802,-58.5119439819544)) ;
#4034 = CARTESIAN_POINT('Ctrl Pts',(-420.576539371367,150.075102689897,-58.5163274770719)) ;
#4035 = CARTESIAN_POINT('Ctrl Pts',(-420.620182438101,150.099058660511,-58.5206631733476)) ;
#4036 = CARTESIAN_POINT('Ctrl Pts',(-420.664247518745,150.122234021346,-58.5249492871398)) ;
#4037 = CARTESIAN_POINT('Ctrl Pts',(-420.485369825263,149.940704294701,-59.0423098699552)) ;
#4038 = CARTESIAN_POINT('Ctrl Pts',(-420.528114397322,149.966191584884,-59.0467393230098)) ;
#4039 = CARTESIAN_POINT('Ctrl Pts',(-420.571320454056,149.990972404078,-59.0507805059011)) ;
#4040 = CARTESIAN_POINT('Ctrl Pts',(-420.61497020581,150.015036144952,-59.0544315754972)) ;
#4041 = CARTESIAN_POINT('Ctrl Pts',(-420.659045309316,150.038373095001,-59.0576911748749)) ;
#4042 = CARTESIAN_POINT('Ctrl Pts',(-420.6241938334,149.627915888419,-59.5024474146452)) ;
#4043 = CARTESIAN_POINT('Ctrl Pts',(-420.666938401923,149.653403185214,-59.5068768636633)) ;
#4044 = CARTESIAN_POINT('Ctrl Pts',(-420.710055598583,149.678384217066,-59.5106235194951)) ;
#4045 = CARTESIAN_POINT('Ctrl Pts',(-420.753527634076,149.702848376139,-59.513685538623)) ;
#4046 = CARTESIAN_POINT('Ctrl Pts',(-420.797336275705,149.726785700566,-59.5160619320858)) ;
#4047 = CARTESIAN_POINT('Ctrl Pts',(-421.013789367829,148.908194055108,-59.884135012707)) ;
#4048 = CARTESIAN_POINT('Ctrl Pts',(-421.056533940723,148.933681343997,-59.8885644652487)) ;
#4049 = CARTESIAN_POINT('Ctrl Pts',(-421.09940176579,148.959123054161,-59.8920668107065)) ;
#4050 = CARTESIAN_POINT('Ctrl Pts',(-421.142375053396,148.984508578293,-59.8946402059013)) ;
#4051 = CARTESIAN_POINT('Ctrl Pts',(-421.185435882405,149.009827379056,-59.8962839664587)) ;
#4052 = CARTESIAN_POINT('Ctrl Pts',(-421.451996513475,148.217919515022,-59.627275259948)) ;
#4053 = CARTESIAN_POINT('Ctrl Pts',(-421.49474108344,148.243406809216,-59.6317047101229)) ;
#4054 = CARTESIAN_POINT('Ctrl Pts',(-421.537328418939,148.269290353584,-59.6353714662152)) ;
#4055 = CARTESIAN_POINT('Ctrl Pts',(-421.579740730352,148.295559540816,-59.63827368484)) ;
#4056 = CARTESIAN_POINT('Ctrl Pts',(-421.621960446587,148.322203282162,-59.6404104766189)) ;
#4057 = CARTESIAN_POINT('Ctrl Pts',(-421.613231704278,147.983523447751,-59.4200694389356)) ;
#4058 = CARTESIAN_POINT('Ctrl Pts',(-421.655976274758,148.00901074047,-59.4244988926215)) ;
#4059 = CARTESIAN_POINT('Ctrl Pts',(-421.698460406657,148.035044317106,-59.4282982785714)) ;
#4060 = CARTESIAN_POINT('Ctrl Pts',(-421.740666310351,148.061613570312,-59.4314657535976)) ;
#4061 = CARTESIAN_POINT('Ctrl Pts',(-421.782576543553,148.088707224125,-59.4340002626073)) ;
#4062 = CARTESIAN_POINT('Ctrl Pts',(-421.736314996746,147.825908589189,-59.1392295361033)) ;
#4063 = CARTESIAN_POINT('Ctrl Pts',(-421.779059567893,147.851395881237,-59.1436589872169)) ;
#4064 = CARTESIAN_POINT('Ctrl Pts',(-421.821464916546,147.87753034417,-59.1476381330355)) ;
#4065 = CARTESIAN_POINT('Ctrl Pts',(-421.863513253218,147.904301370467,-59.1511651300512)) ;
#4066 = CARTESIAN_POINT('Ctrl Pts',(-421.905187233809,147.931697558431,-59.1542386991413)) ;
#4067 = CARTESIAN_POINT('Ctrl Pts',(-421.811062973951,147.754793329066,-58.8271062522543)) ;
#4068 = CARTESIAN_POINT('Ctrl Pts',(-421.8538075451,147.780280621111,-58.8315357033629)) ;
#4069 = CARTESIAN_POINT('Ctrl Pts',(-421.89616504891,147.806460603649,-58.835714633705)) ;
#4070 = CARTESIAN_POINT('Ctrl Pts',(-421.938117695878,147.833322669176,-58.8396411998575)) ;
#4071 = CARTESIAN_POINT('Ctrl Pts',(-421.979648201636,147.860855359163,-58.8433138732736)) ;
#4072 = CARTESIAN_POINT('Origin',(-421.377235834177,148.938878434349,-58.4534262754551)) ;
#4073 = CARTESIAN_POINT('Origin',(-428.991534950723,153.479054187111,-59.2424660232112)) ;
#4074 = CARTESIAN_POINT('',(-423.25286169586,147.847682592174,-57.9134552983687)) ;
#4075 = CARTESIAN_POINT('',(-421.302624061803,151.113877299569,-57.939556238929)) ;
#4076 = CARTESIAN_POINT('Origin',(-422.232863749181,149.44906342357,-58.542091617402)) ;
#4077 = CARTESIAN_POINT('',(-428.061295263345,155.143868063109,-58.6399306447382)) ;
#4078 = CARTESIAN_POINT('Origin',(-422.232863749181,149.44906342357,-58.542091617402)) ;
#4079 = CARTESIAN_POINT('Origin',(-422.232863749181,149.44906342357,-58.542091617402)) ;
#4080 = CARTESIAN_POINT('',(-421.129412046089,151.016134561919,-57.9203439835838)) ;
#4081 = CARTESIAN_POINT('',(-423.084516151496,147.741789646215,-57.8941779127654)) ;
#4082 = CARTESIAN_POINT('Origin',(-422.061972981251,149.347166438823,-58.5243828819896)) ;
#4083 = CARTESIAN_POINT('Origin',(-425.292857589218,144.644920929381,-56.6561826603022)) ;
#4084 = CARTESIAN_POINT('Origin',(-422.061972981251,149.347166438823,-58.5243828819896)) ;
#4085 = CARTESIAN_POINT('Origin',(-428.991534950723,153.479054187111,-59.2424660232112)) ;
#4086 = CARTESIAN_POINT('',(-420.236817124951,150.533858084077,-57.816462643087)) ;
#4087 = CARTESIAN_POINT('',(-428.038039271161,155.185488410009,-58.6248672602764)) ;
#4088 = CARTESIAN_POINT('',(-422.143809736987,147.120988422025,-59.0516550729336)) ;
#4089 = CARTESIAN_POINT('Origin',(-421.190314057423,148.827422644927,-58.4340563099994)) ;
#4090 = CARTESIAN_POINT('Origin',(-421.190314057423,148.827422644927,-58.4340563099994)) ;
#4091 = CARTESIAN_POINT('Origin',(-422.147365028502,149.39808312813,-58.5332317226227)) ;
#4092 = CARTESIAN_POINT('',(-422.343986042163,147.246924259843,-59.0708987663161)) ;
#4093 = CARTESIAN_POINT('',(-420.442506399576,150.649927582747,-57.8392771818555)) ;
#4094 = CARTESIAN_POINT('Origin',(-421.393246844343,148.948425314316,-58.4550854333019)) ;
#4095 = CARTESIAN_POINT('Origin',(-421.393246844343,148.948425314316,-58.4550854333019)) ;
#4096 = CARTESIAN_POINT('',(-421.217125341124,151.062897004128,-57.9306963441498)) ;
#4097 = CARTESIAN_POINT('Ctrl Pts',(-420.442317319748,150.650212478691,-57.8403702955082)) ;
#4098 = CARTESIAN_POINT('Ctrl Pts',(-420.390229898959,150.622444850762,-57.8342240564197)) ;
#4099 = CARTESIAN_POINT('Ctrl Pts',(-420.338559599104,150.593830011908,-57.8283703755451)) ;
#4100 = CARTESIAN_POINT('Ctrl Pts',(-420.287328108581,150.564379524318,-57.8228118120409)) ;
#4101 = CARTESIAN_POINT('Ctrl Pts',(-420.236556568021,150.534105993319,-57.8175505566696)) ;
#4102 = CARTESIAN_POINT('Ctrl Pts',(-420.626777418833,150.474826238209,-57.069496565559)) ;
#4103 = CARTESIAN_POINT('Ctrl Pts',(-420.574957527116,150.446804241574,-57.0622322995815)) ;
#4104 = CARTESIAN_POINT('Ctrl Pts',(-420.523465654325,150.418019752801,-57.0556329570686)) ;
#4105 = CARTESIAN_POINT('Ctrl Pts',(-420.472323377486,150.388484440006,-57.049701562745)) ;
#4106 = CARTESIAN_POINT('Ctrl Pts',(-420.42155183722,150.358210908514,-57.0444403073611)) ;
#4107 = CARTESIAN_POINT('Ctrl Pts',(-420.998424490206,149.96520818523,-56.4154402406386)) ;
#4108 = CARTESIAN_POINT('Ctrl Pts',(-420.94714361401,149.936447067719,-56.4072273700832)) ;
#4109 = CARTESIAN_POINT('Ctrl Pts',(-420.896011233862,149.907169627505,-56.3999953620422)) ;
#4110 = CARTESIAN_POINT('Ctrl Pts',(-420.845048702436,149.877387840324,-56.3937476359878)) ;
#4111 = CARTESIAN_POINT('Ctrl Pts',(-420.794277160261,149.847114311642,-56.3884863828677)) ;
#4112 = CARTESIAN_POINT('Ctrl Pts',(-421.500791590854,149.167595269917,-56.1570621835743)) ;
#4113 = CARTESIAN_POINT('Ctrl Pts',(-421.450239313169,149.137677350129,-56.1484745773338)) ;
#4114 = CARTESIAN_POINT('Ctrl Pts',(-421.399592868659,149.107628385508,-56.1409926414793)) ;
#4115 = CARTESIAN_POINT('Ctrl Pts',(-421.348873306703,149.077460833301,-56.1346199518746)) ;
#4116 = CARTESIAN_POINT('Ctrl Pts',(-421.298101767752,149.047187299145,-56.129358699136)) ;
#4117 = CARTESIAN_POINT('Ctrl Pts',(-422.182013907982,147.96033734627,-56.529835127009)) ;
#4118 = CARTESIAN_POINT('Ctrl Pts',(-422.132449635391,147.928668489913,-56.5217881696355)) ;
#4119 = CARTESIAN_POINT('Ctrl Pts',(-422.082462134238,147.897451749959,-56.5146668157615)) ;
#4120 = CARTESIAN_POINT('Ctrl Pts',(-422.032072042464,147.866700312821,-56.5084744157967)) ;
#4121 = CARTESIAN_POINT('Ctrl Pts',(-421.981300500553,147.836426784044,-56.5032131606753)) ;
#4122 = CARTESIAN_POINT('Ctrl Pts',(-422.464086691705,147.292074351448,-57.6530293612976)) ;
#4123 = CARTESIAN_POINT('Ctrl Pts',(-422.414931518073,147.259436291465,-57.6466114130534)) ;
#4124 = CARTESIAN_POINT('Ctrl Pts',(-422.365216863686,147.227573145683,-57.640576517863)) ;
#4125 = CARTESIAN_POINT('Ctrl Pts',(-422.314963196154,147.196498504072,-57.6349273479934)) ;
#4126 = CARTESIAN_POINT('Ctrl Pts',(-422.264191655957,147.166224972182,-57.6296660942382)) ;
#4127 = CARTESIAN_POINT('Ctrl Pts',(-422.49553424485,147.155810241822,-58.1336286388597)) ;
#4128 = CARTESIAN_POINT('Ctrl Pts',(-422.446424681794,147.122974551427,-58.127907720542)) ;
#4129 = CARTESIAN_POINT('Ctrl Pts',(-422.396740446769,147.090979597685,-58.1223377058509)) ;
#4130 = CARTESIAN_POINT('Ctrl Pts',(-422.346501988429,147.059839052819,-58.1169209767701)) ;
#4131 = CARTESIAN_POINT('Ctrl Pts',(-422.295730447237,147.029565522422,-58.1116597241416)) ;
#4132 = CARTESIAN_POINT('Ctrl Pts',(-422.451413471441,147.144684274654,-58.623417159732)) ;
#4133 = CARTESIAN_POINT('Ctrl Pts',(-422.402239917998,147.111832448195,-58.6184066016194)) ;
#4134 = CARTESIAN_POINT('Ctrl Pts',(-422.352513005096,147.079826732491,-58.613310356972)) ;
#4135 = CARTESIAN_POINT('Ctrl Pts',(-422.302253207981,147.048680806466,-58.6081305121877)) ;
#4136 = CARTESIAN_POINT('Ctrl Pts',(-422.251481667166,147.018407275726,-58.6028692579116)) ;
#4137 = CARTESIAN_POINT('Ctrl Pts',(-422.343792618447,147.247216634306,-59.0719908009918)) ;
#4138 = CARTESIAN_POINT('Ctrl Pts',(-422.294462978472,147.214513514342,-59.0676308259597)) ;
#4139 = CARTESIAN_POINT('Ctrl Pts',(-422.244631964546,147.182606977597,-59.0629684839705)) ;
#4140 = CARTESIAN_POINT('Ctrl Pts',(-422.194320116926,147.151510641041,-59.0580055905041)) ;
#4141 = CARTESIAN_POINT('Ctrl Pts',(-422.143548576108,147.121237110302,-59.0527443362252)) ;
#4142 = CARTESIAN_POINT('Origin',(-422.446249450215,146.579713262273,-59.2475425158174)) ;
#4143 = CARTESIAN_POINT('Origin',(-419.934490494852,151.074921350906,-57.6206335614338)) ;
#4144 = CARTESIAN_POINT('Ctrl Pts',(-422.34418631909,147.246799897813,-59.070237373874)) ;
#4145 = CARTESIAN_POINT('Ctrl Pts',(-422.294863584558,147.214100818998,-59.0658753144168)) ;
#4146 = CARTESIAN_POINT('Ctrl Pts',(-422.245039410828,147.182198310169,-59.0612118137456)) ;
#4147 = CARTESIAN_POINT('Ctrl Pts',(-422.194734329872,147.151105983027,-59.0562486877295)) ;
#4148 = CARTESIAN_POINT('Ctrl Pts',(-422.143969473837,147.120836438223,-59.0509881261684)) ;
#4149 = CARTESIAN_POINT('Ctrl Pts',(-422.228145324003,147.357174965478,-59.554938735971)) ;
#4150 = CARTESIAN_POINT('Ctrl Pts',(-422.178654335311,147.324635925487,-59.5512794714222)) ;
#4151 = CARTESIAN_POINT('Ctrl Pts',(-422.128717945445,147.292840153624,-59.5470846957269)) ;
#4152 = CARTESIAN_POINT('Ctrl Pts',(-422.078356756426,147.261801194959,-59.5423559321871)) ;
#4153 = CARTESIAN_POINT('Ctrl Pts',(-422.027591900393,147.231531650153,-59.5370953706258)) ;
#4154 = CARTESIAN_POINT('Ctrl Pts',(-422.037973303002,147.600208882302,-59.9916847370896)) ;
#4155 = CARTESIAN_POINT('Ctrl Pts',(-421.98820657396,147.56802223003,-59.9886587324345)) ;
#4156 = CARTESIAN_POINT('Ctrl Pts',(-421.938086280561,147.536461481207,-59.9848863063301)) ;
#4157 = CARTESIAN_POINT('Ctrl Pts',(-421.88763313952,147.505540034306,-59.9803687186285)) ;
#4158 = CARTESIAN_POINT('Ctrl Pts',(-421.836868283048,147.475270489885,-59.9751081589749)) ;
#4159 = CARTESIAN_POINT('Ctrl Pts',(-421.789025698594,147.961261985461,-60.3165314648779)) ;
#4160 = CARTESIAN_POINT('Ctrl Pts',(-421.738898007252,147.92959884269,-60.3139764756352)) ;
#4161 = CARTESIAN_POINT('Ctrl Pts',(-421.688536972012,147.898387245812,-60.310518189728)) ;
#4162 = CARTESIAN_POINT('Ctrl Pts',(-421.637963459867,147.867640375442,-60.3061576708561)) ;
#4163 = CARTESIAN_POINT('Ctrl Pts',(-421.587198603022,147.837370832091,-60.3008971087469)) ;
#4164 = CARTESIAN_POINT('Ctrl Pts',(-421.102314662438,149.040189908199,-60.7351426238331)) ;
#4165 = CARTESIAN_POINT('Ctrl Pts',(-421.051191269308,149.010091165465,-60.7331946003715)) ;
#4166 = CARTESIAN_POINT('Ctrl Pts',(-421.000166157263,148.97992293485,-60.7301411271694)) ;
#4167 = CARTESIAN_POINT('Ctrl Pts',(-420.94926060771,148.949697745786,-60.7259830153771)) ;
#4168 = CARTESIAN_POINT('Ctrl Pts',(-420.898495752919,148.919428198737,-60.7207224546085)) ;
#4169 = CARTESIAN_POINT('Ctrl Pts',(-420.483542510817,150.179465060839,-60.1508967990536)) ;
#4170 = CARTESIAN_POINT('Ctrl Pts',(-420.431521929361,150.151018209618,-60.1481016477795)) ;
#4171 = CARTESIAN_POINT('Ctrl Pts',(-420.379898441695,150.121951700366,-60.1444831869925)) ;
#4172 = CARTESIAN_POINT('Ctrl Pts',(-420.328693702851,150.092277374683,-60.1400425803007)) ;
#4173 = CARTESIAN_POINT('Ctrl Pts',(-420.27792884495,150.062007833199,-60.1347820175111)) ;
#4174 = CARTESIAN_POINT('Ctrl Pts',(-420.259174590128,150.682575177394,-59.4211440937216)) ;
#4175 = CARTESIAN_POINT('Ctrl Pts',(-420.206828682934,150.654857817706,-59.4172908307359)) ;
#4176 = CARTESIAN_POINT('Ctrl Pts',(-420.154988222027,150.626277836902,-59.4129666696233)) ;
#4177 = CARTESIAN_POINT('Ctrl Pts',(-420.103674997724,150.596846773186,-59.4081732146125)) ;
#4178 = CARTESIAN_POINT('Ctrl Pts',(-420.052910142311,150.566577226921,-59.4029126553418)) ;
#4179 = CARTESIAN_POINT('Ctrl Pts',(-420.266515670992,150.817595489973,-58.5733881509068)) ;
#4180 = CARTESIAN_POINT('Ctrl Pts',(-420.214180408597,150.790073902018,-58.5683056838671)) ;
#4181 = CARTESIAN_POINT('Ctrl Pts',(-420.162347047,150.761624490549,-58.5631617112019)) ;
#4182 = CARTESIAN_POINT('Ctrl Pts',(-420.111037372064,150.732258712297,-58.5579583485471)) ;
#4183 = CARTESIAN_POINT('Ctrl Pts',(-420.060272516065,150.701989167613,-58.5526977858246)) ;
#4184 = CARTESIAN_POINT('Ctrl Pts',(-420.442710151574,150.649797874219,-57.8386129852327)) ;
#4185 = CARTESIAN_POINT('Ctrl Pts',(-420.390630362941,150.622032987744,-57.8324651274969)) ;
#4186 = CARTESIAN_POINT('Ctrl Pts',(-420.33896738815,150.593421309605,-57.8266105987488)) ;
#4187 = CARTESIAN_POINT('Ctrl Pts',(-420.287742906723,150.563974397833,-57.8210519581525)) ;
#4188 = CARTESIAN_POINT('Ctrl Pts',(-420.236978050927,150.533704852778,-57.8157913956035)) ;
#4189 = CARTESIAN_POINT('Origin',(-428.991534950723,153.479054187111,-59.2424660232112)) ;
#4190 = CARTESIAN_POINT('',(-421.667494954702,150.499130901467,-58.167168236128)) ;
#4191 = CARTESIAN_POINT('',(-428.410135146112,154.51956285961,-58.8658814116656)) ;
#4192 = CARTESIAN_POINT('Origin',(-422.248894759313,149.458622228968,-58.5437528476736)) ;
#4193 = CARTESIAN_POINT('Origin',(-422.147365028502,149.39808312813,-58.5332317226227)) ;
#4194 = CARTESIAN_POINT('',(-421.461805686039,150.383061400504,-58.1443536829051)) ;
#4195 = CARTESIAN_POINT('Origin',(-422.045961972393,149.337619559579,-58.522723724371)) ;
#4196 = CARTESIAN_POINT('',(-421.565965223891,150.438591800629,-58.1566471110771)) ;
#4197 = CARTESIAN_POINT('Origin',(-422.248894759313,149.458622228968,-58.5437528476736)) ;
#4198 = CARTESIAN_POINT('Origin',(-419.45817569718,154.453063856963,-56.7361467122547)) ;
#4199 = CARTESIAN_POINT('',(0.,0.,0.)) ;
#4200 = CARTESIAN_POINT('Origin',(0.,-7.25000000007,0.)) ;
#4201 = CARTESIAN_POINT('',(1.96564470827723,-11.5,-3.59808850375053)) ;
#4202 = CARTESIAN_POINT('Origin',(0.,-11.5,0.)) ;
#4203 = CARTESIAN_POINT('',(1.96564470827723,-17.,-3.59808850375053)) ;
#4204 = CARTESIAN_POINT('',(1.96564470827723,-7.25000000007,-3.59808850375053)) ;
#4205 = CARTESIAN_POINT('Origin',(0.,-17.,0.)) ;
#4206 = CARTESIAN_POINT('Origin',(0.,-10.4,0.)) ;
#4207 = CARTESIAN_POINT('',(1.43827661581261,-10.4,-2.63274768567112)) ;
#4208 = CARTESIAN_POINT('Origin',(0.,-10.4,0.)) ;
#4209 = CARTESIAN_POINT('',(1.43827661581261,-10.4,-2.63274768567112)) ;
#4210 = CARTESIAN_POINT('Origin',(0.,-7.25000000007,0.)) ;
#4211 = CARTESIAN_POINT('',(1.43827661581261,-6.19238815543,-2.63274768567112)) ;
#4212 = CARTESIAN_POINT('Origin',(0.,-6.19238815543,0.)) ;
#4213 = CARTESIAN_POINT('',(1.43827661581261,-7.25000000007,-2.63274768567112)) ;
#4214 = CARTESIAN_POINT('Origin',(0.,-6.19238815543,0.)) ;
#4215 = CARTESIAN_POINT('',(2.20353282123762,-4.59619407771428,-4.03353977366586)) ;
#4216 = CARTESIAN_POINT('',(1.43827661581261,-6.19238815543,-2.63274768567112)) ;
#4217 = CARTESIAN_POINT('Origin',(0.,-4.59619407771,0.)) ;
#4218 = CARTESIAN_POINT('Origin',(0.,0.,0.)) ;
#4219 = CARTESIAN_POINT('',(2.94914909303845,2.1,-5.39838120430629)) ;
#4220 = CARTESIAN_POINT('Origin',(0.,2.1,0.)) ;
#4221 = CARTESIAN_POINT('Origin',(0.,0.,0.)) ;
#4222 = CARTESIAN_POINT('Origin',(0.,-17.,4.1)) ;
#4223 = CARTESIAN_POINT('',(-0.788217635939279,-17.,5.73886432473532)) ;
#4224 = CARTESIAN_POINT('Origin',(-8.881784197E-16,-17.,-1.7763568394E-15)) ;
#4225 = CARTESIAN_POINT('Origin',(8.881784197E-16,-16.7,2.22044604925E-16)) ;
#4226 = CARTESIAN_POINT('',(-0.826357198968776,-16.8069360227,6.01655130819153)) ;
#4227 = CARTESIAN_POINT('Origin',(-0.78821763593928,-16.7,5.73886432473532)) ;
#4228 = CARTESIAN_POINT('',(2.91156814503746,-16.8069360227,-5.32958974042017)) ;
#4229 = CARTESIAN_POINT('Origin',(8.881784197E-16,-16.8069360227,2.22044604925E-16)) ;
#4230 = CARTESIAN_POINT('Origin',(8.881784197E-16,-16.8069360227,2.22044604925E-16)) ;
#4231 = CARTESIAN_POINT('Origin',(0.,-14.4899888641,5.93873487707E-17)) ;
#4232 = CARTESIAN_POINT('',(2.29137205950736,-10.0846258617,-4.19432842080319)) ;
#4233 = CARTESIAN_POINT('Origin',(0.,-14.4899888641,5.93873487707E-17)) ;
#4234 = CARTESIAN_POINT('',(0.611605452441915,-10.0846258617,4.74011767651307)) ;
#4235 = CARTESIAN_POINT('Origin',(0.,-10.0846258617,5.93873487707E-17)) ;
#4236 = CARTESIAN_POINT('Origin',(0.,-10.0846258617,5.93873487707E-17)) ;
#4237 = CARTESIAN_POINT('Origin',(1.11022302463E-15,-9.88130141541,4.4408920985E-16)) ;
#4238 = CARTESIAN_POINT('',(0.601443392616207,-9.88130141541,4.66135879819161)) ;
#4239 = CARTESIAN_POINT('Origin',(0.639833396400221,-9.88130141541,4.95889233850171)) ;
#4240 = CARTESIAN_POINT('',(2.25330003143976,-9.88130141541,-4.12463804088475)) ;
#4241 = CARTESIAN_POINT('Origin',(1.11022302463E-15,-9.88130141541,4.4408920985E-16)) ;
#4242 = CARTESIAN_POINT('Origin',(1.11022302463E-15,-9.88130141541,4.4408920985E-16)) ;
#4243 = CARTESIAN_POINT('Origin',(0.,-7.25000000007,0.)) ;
#4244 = CARTESIAN_POINT('',(2.25330003143976,-9.17835096162,-4.12463804088475)) ;
#4245 = CARTESIAN_POINT('',(2.25330003143976,-7.25000000007,-4.12463804088475)) ;
#4246 = CARTESIAN_POINT('',(0.601443392616206,-9.17835096162,4.66135879819161)) ;
#4247 = CARTESIAN_POINT('Origin',(0.,-9.17835096162,0.)) ;
#4248 = CARTESIAN_POINT('Origin',(0.,-9.17835096162,0.)) ;
#4249 = CARTESIAN_POINT('Origin',(-4.4408920985E-16,-9.17835096162,0.)) ;
#4250 = CARTESIAN_POINT('',(0.609333419211508,-8.83264560279,4.72250876731505)) ;
#4251 = CARTESIAN_POINT('Origin',(0.72941007189625,-9.17835096162,5.65313726589195)) ;
#4252 = CARTESIAN_POINT('',(2.2828599158681,-8.83264560279086,-4.17874704638608)) ;
#4253 = CARTESIAN_POINT('Origin',(-4.4408920985E-16,-8.83264560279,0.)) ;
#4254 = CARTESIAN_POINT('Origin',(-4.4408920985E-16,-8.83264560279,0.)) ;
#4255 = CARTESIAN_POINT('Origin',(1.7763568394E-15,2.2,8.881784197E-16)) ;
#4256 = CARTESIAN_POINT('',(3.93128941655447,2.2,-7.19617700750105)) ;
#4257 = CARTESIAN_POINT('',(-3.32258683237438,2.2,7.49669372065662)) ;
#4258 = CARTESIAN_POINT('Origin',(-4.4408920985E-15,2.2,-2.6645352591E-15)) ;
#4259 = CARTESIAN_POINT('Origin',(-4.4408920985E-15,2.2,-2.6645352591E-15)) ;
#4260 = CARTESIAN_POINT('',(-3.20102877753141,2.5,7.22242443819357)) ;
#4261 = CARTESIAN_POINT('Origin',(-3.20102877753141,2.2,7.22242443819357)) ;
#4262 = CARTESIAN_POINT('Origin',(1.7763568394E-15,2.5,8.881784197E-16)) ;
#4263 = CARTESIAN_POINT('Origin',(0.,-9.,0.)) ;
#4264 = CARTESIAN_POINT('',(3.90172953212637,0.332645602789664,-7.14206800200019)) ;
#4265 = CARTESIAN_POINT('Origin',(0.,0.332645602789,0.)) ;
#4266 = CARTESIAN_POINT('',(2.25330003143976,-9.,-4.12463804088475)) ;
#4267 = CARTESIAN_POINT('Origin',(0.,-7.25000000007,0.)) ;
#4268 = CARTESIAN_POINT('',(3.93128941655,0.678350961617,-7.1961770075)) ;
#4269 = CARTESIAN_POINT('Origin',(0.,0.678350961617,0.)) ;
#4270 = CARTESIAN_POINT('',(3.93128941655446,-7.25000000007,-7.19617700750106)) ;
#4271 = CARTESIAN_POINT('Origin',(4.4408920985E-16,0.678350961617,8.881784197E-16)) ;
#4272 = CARTESIAN_POINT('Origin',(3.45186387795027,0.678350961617,-6.31859444561068)) ;
#4273 = CARTESIAN_POINT('Origin',(0.,-7.25000000007,0.)) ;
#4274 = CARTESIAN_POINT('',(2.94914909304,2.3,-5.39838120431)) ;
#4275 = CARTESIAN_POINT('Origin',(0.,2.3,0.)) ;
#4276 = CARTESIAN_POINT('',(2.94914909303845,-7.25000000007,-5.39838120430628)) ;
#4277 = CARTESIAN_POINT('Origin',(0.,2.5,8.2)) ;
#4278 = CARTESIAN_POINT('',(3.04503425308,2.5,-5.57389768811)) ;
#4279 = CARTESIAN_POINT('Origin',(3.21964677141E-15,2.5,-5.3290705182E-15)) ;
#4280 = CARTESIAN_POINT('Origin',(1.7763568394E-15,2.3,1.11022302463E-15)) ;
#4281 = CARTESIAN_POINT('Origin',(3.0450342007593,2.3,-5.57389771668436)) ;
#4282 = CARTESIAN_POINT('',(-458.263628686457,237.190054016881,-23.7000000000077)) ;
#4283 = CARTESIAN_POINT('',(0.,0.,0.)) ;
#4284 = CARTESIAN_POINT('',(0.,0.,0.)) ;
#4285 = CARTESIAN_POINT('',(0.,0.,0.)) ;
#4286 = CARTESIAN_POINT('',(-458.263628686547,222.700065152751,-23.6999999999751)) ;
#4287 = CARTESIAN_POINT('',(-471.230319587396,218.286733435889,-18.9727166870646)) ;
#4288 = CARTESIAN_POINT('',(-474.821799069225,206.896169362749,-27.1773557716937)) ;
#4289 = CARTESIAN_POINT('',(-483.667771242974,202.019941589869,-37.5663382189789)) ;
#4290 = CARTESIAN_POINT('',(-473.797618531234,192.990302277591,-43.1345943752389)) ;
#4291 = CARTESIAN_POINT('',(-464.616569660766,183.350302780878,-48.8563535997431)) ;
#4292 = CARTESIAN_POINT('',(-455.435520790299,173.710303284165,-54.5781128242473)) ;
#4293 = UNCERTAINTY_MEASURE_WITH_UNIT(LENGTH_MEASURE(0.01),#4305,
'DISTANCE_ACCURACY_VALUE',
'Maximum model space distance between geometric entities at asserted c
onnectivities') ;
#4294 = UNCERTAINTY_MEASURE_WITH_UNIT(LENGTH_MEASURE(0.01),#4305,
'DISTANCE_ACCURACY_VALUE',
'Maximum model space distance between geometric entities at asserted c
onnectivities') ;
#4295 = UNCERTAINTY_MEASURE_WITH_UNIT(LENGTH_MEASURE(0.01),#4305,
'DISTANCE_ACCURACY_VALUE',
'Maximum model space distance between geometric entities at asserted c
onnectivities') ;
#4296 = UNCERTAINTY_MEASURE_WITH_UNIT(LENGTH_MEASURE(0.01),#4305,
'DISTANCE_ACCURACY_VALUE',
'Maximum model space distance between geometric entities at asserted c
onnectivities') ;
#4297 = UNCERTAINTY_MEASURE_WITH_UNIT(LENGTH_MEASURE(0.01),#4305,
'DISTANCE_ACCURACY_VALUE',
'Maximum model space distance between geometric entities at asserted c
onnectivities') ;
#4298 = UNCERTAINTY_MEASURE_WITH_UNIT(LENGTH_MEASURE(0.01),#4305,
'DISTANCE_ACCURACY_VALUE',
'Maximum model space distance between geometric entities at asserted c
onnectivities') ;
#4299 = (
GEOMETRIC_REPRESENTATION_CONTEXT(3)
GLOBAL_UNCERTAINTY_ASSIGNED_CONTEXT((#4293))
GLOBAL_UNIT_ASSIGNED_CONTEXT((#4305,#4307,#4308))
REPRESENTATION_CONTEXT('','3D')
) ;
#4300 = (
GEOMETRIC_REPRESENTATION_CONTEXT(3)
GLOBAL_UNCERTAINTY_ASSIGNED_CONTEXT((#4294))
GLOBAL_UNIT_ASSIGNED_CONTEXT((#4305,#4307,#4308))
REPRESENTATION_CONTEXT('','3D')
) ;
#4301 = (
GEOMETRIC_REPRESENTATION_CONTEXT(3)
GLOBAL_UNCERTAINTY_ASSIGNED_CONTEXT((#4295))
GLOBAL_UNIT_ASSIGNED_CONTEXT((#4305,#4307,#4308))
REPRESENTATION_CONTEXT('','3D')
) ;
#4302 = (
GEOMETRIC_REPRESENTATION_CONTEXT(3)
GLOBAL_UNCERTAINTY_ASSIGNED_CONTEXT((#4296))
GLOBAL_UNIT_ASSIGNED_CONTEXT((#4305,#4307,#4308))
REPRESENTATION_CONTEXT('','3D')
) ;
#4303 = (
GEOMETRIC_REPRESENTATION_CONTEXT(3)
GLOBAL_UNCERTAINTY_ASSIGNED_CONTEXT((#4297))
GLOBAL_UNIT_ASSIGNED_CONTEXT((#4305,#4307,#4308))
REPRESENTATION_CONTEXT('','3D')
) ;
#4304 = (
GEOMETRIC_REPRESENTATION_CONTEXT(3)
GLOBAL_UNCERTAINTY_ASSIGNED_CONTEXT((#4298))
GLOBAL_UNIT_ASSIGNED_CONTEXT((#4305,#4307,#4308))
REPRESENTATION_CONTEXT('','3D')
) ;
#4305 = (
LENGTH_UNIT()
NAMED_UNIT(*)
SI_UNIT(.MILLI.,.METRE.)
) ;
#4306 = (
LENGTH_UNIT()
NAMED_UNIT(*)
SI_UNIT($,.METRE.)
) ;
#4307 = (
NAMED_UNIT(*)
PLANE_ANGLE_UNIT()
SI_UNIT($,.RADIAN.)
) ;
#4308 = (
NAMED_UNIT(*)
SI_UNIT($,.STERADIAN.)
SOLID_ANGLE_UNIT()
) ;
#4309 = SHAPE_DEFINITION_REPRESENTATION(#4314,#4330) ;
#4310 = SHAPE_DEFINITION_REPRESENTATION(#4315,#4331) ;
#4311 = SHAPE_DEFINITION_REPRESENTATION(#4316,#4332) ;
#4312 = SHAPE_DEFINITION_REPRESENTATION(#4317,#4333) ;
#4313 = SHAPE_DEFINITION_REPRESENTATION(#4318,#4334) ;
#4314 = PRODUCT_DEFINITION_SHAPE('',$,#4336) ;
#4315 = PRODUCT_DEFINITION_SHAPE('',$,#4337) ;
#4316 = PRODUCT_DEFINITION_SHAPE('',$,#4338) ;
#4317 = PRODUCT_DEFINITION_SHAPE('',$,#4339) ;
#4318 = PRODUCT_DEFINITION_SHAPE('',$,#4340) ;
#4319 = PRODUCT_DEFINITION_SHAPE($,$,#44) ;
#4320 = PRODUCT_DEFINITION_SHAPE($,$,#45) ;
#4321 = PRODUCT_DEFINITION_SHAPE($,$,#46) ;
#4322 = PRODUCT_DEFINITION_SHAPE($,$,#47) ;
#4323 = PRODUCT_DEFINITION_SHAPE($,$,#48) ;
#4324 = PRODUCT_DEFINITION_SHAPE($,$,#49) ;
#4325 = PRODUCT_DEFINITION_SHAPE($,$,#50) ;
#4326 = PRODUCT_DEFINITION_SHAPE($,$,#51) ;
#4327 = PRODUCT_DEFINITION_SHAPE($,$,#52) ;
#4328 = PRODUCT_DEFINITION_SHAPE($,$,#53) ;
#4329 = PRODUCT_DEFINITION_SHAPE($,$,#54) ;
#4330 = SHAPE_REPRESENTATION('',(#2213,#2519,#2520,#2521,#2522,#2523,#2524,
#2525,#2526,#2527,#2528,#2529),#4299) ;
#4331 = SHAPE_REPRESENTATION('',(#2214),#4300) ;
#4332 = SHAPE_REPRESENTATION('',(#2268),#4301) ;
#4333 = SHAPE_REPRESENTATION('',(#2366),#4302) ;
#4334 = SHAPE_REPRESENTATION('',(#2468),#4303) ;
#4335 = PRODUCT_DEFINITION_CONTEXT('part definition',#4352,'design') ;
#4336 = PRODUCT_DEFINITION('MAS-656','MAS-656',#4341,#4335) ;
#4337 = PRODUCT_DEFINITION('Conjunction','Conjunction',#4342,#4335) ;
#4338 = PRODUCT_DEFINITION('Connector_1-8','Connector_1-8',#4343,#4335) ;
#4339 = PRODUCT_DEFINITION('Nozzle','Nozzle',#4344,#4335) ;
#4340 = PRODUCT_DEFINITION('Segment','Segment',#4345,#4335) ;
#4341 = PRODUCT_DEFINITION_FORMATION('',$,#4354) ;
#4342 = PRODUCT_DEFINITION_FORMATION('',$,#4355) ;
#4343 = PRODUCT_DEFINITION_FORMATION('',$,#4356) ;
#4344 = PRODUCT_DEFINITION_FORMATION('',$,#4357) ;
#4345 = PRODUCT_DEFINITION_FORMATION('',$,#4358) ;
#4346 = PRODUCT_RELATED_PRODUCT_CATEGORY('MAS-656','MAS-656',(#4354)) ;
#4347 = PRODUCT_RELATED_PRODUCT_CATEGORY('Conjunction','Conjunction',(#4355)) ;
#4348 = PRODUCT_RELATED_PRODUCT_CATEGORY('Connector_1-8','Connector_1-8',
(#4356)) ;
#4349 = PRODUCT_RELATED_PRODUCT_CATEGORY('Nozzle','Nozzle',(#4357)) ;
#4350 = PRODUCT_RELATED_PRODUCT_CATEGORY('Segment','Segment',(#4358)) ;
#4351 = APPLICATION_PROTOCOL_DEFINITION('international standard',
'automotive_design',2009,#4352) ;
#4352 = APPLICATION_CONTEXT(
'Core Data for Automotive Mechanical Design Process') ;
#4353 = PRODUCT_CONTEXT('part definition',#4352,'mechanical') ;
#4354 = PRODUCT('MAS-656','MAS-656',$,(#4353)) ;
#4355 = PRODUCT('Conjunction','Conjunction',$,(#4353)) ;
#4356 = PRODUCT('Connector_1-8','Connector_1-8',$,(#4353)) ;
#4357 = PRODUCT('Nozzle','Nozzle',$,(#4353)) ;
#4358 = PRODUCT('Segment','Segment',$,(#4353)) ;
#4359 = PRESENTATION_STYLE_ASSIGNMENT((#4363)) ;
#4360 = PRESENTATION_STYLE_ASSIGNMENT((#4364)) ;
#4361 = PRESENTATION_STYLE_ASSIGNMENT((#4365)) ;
#4362 = PRESENTATION_STYLE_ASSIGNMENT((#4366)) ;
#4363 = SURFACE_STYLE_USAGE(.BOTH.,#4367) ;
#4364 = SURFACE_STYLE_USAGE(.BOTH.,#4368) ;
#4365 = SURFACE_STYLE_USAGE(.BOTH.,#4369) ;
#4366 = SURFACE_STYLE_USAGE(.BOTH.,#4370) ;
#4367 = SURFACE_SIDE_STYLE('',(#4371)) ;
#4368 = SURFACE_SIDE_STYLE('',(#4372)) ;
#4369 = SURFACE_SIDE_STYLE('',(#4373)) ;
#4370 = SURFACE_SIDE_STYLE('',(#4374)) ;
#4371 = SURFACE_STYLE_FILL_AREA(#4375) ;
#4372 = SURFACE_STYLE_FILL_AREA(#4376) ;
#4373 = SURFACE_STYLE_FILL_AREA(#4377) ;
#4374 = SURFACE_STYLE_FILL_AREA(#4378) ;
#4375 = FILL_AREA_STYLE('Steel - Satin',(#4379)) ;
#4376 = FILL_AREA_STYLE('Opaque(243,203,124)',(#4380)) ;
#4377 = FILL_AREA_STYLE('Opaque(210,210,255)',(#4381)) ;
#4378 = FILL_AREA_STYLE('Opaque(48,59,150)',(#4382)) ;
#4379 = FILL_AREA_STYLE_COLOUR('Steel - Satin',#4383) ;
#4380 = FILL_AREA_STYLE_COLOUR('Opaque(243,203,124)',#4384) ;
#4381 = FILL_AREA_STYLE_COLOUR('Opaque(210,210,255)',#4385) ;
#4382 = FILL_AREA_STYLE_COLOUR('Opaque(48,59,150)',#4386) ;
#4383 = COLOUR_RGB('Steel - Satin', 0.09019608, 0.27058824, 0.51372549) ;
#4384 = COLOUR_RGB('Opaque(243,203,124)', 0.09019608, 0.27058824, 0.51372549) ;
#4385 = COLOUR_RGB('Opaque(210,210,255)', 0.72549020, 0.75294118, 0.79215686) ;
#4386 = COLOUR_RGB('Opaque(48,59,150)', 0.08235294, 0.09019608, 0.10196078) ;
ENDSEC;
END-ISO-10303-21;
